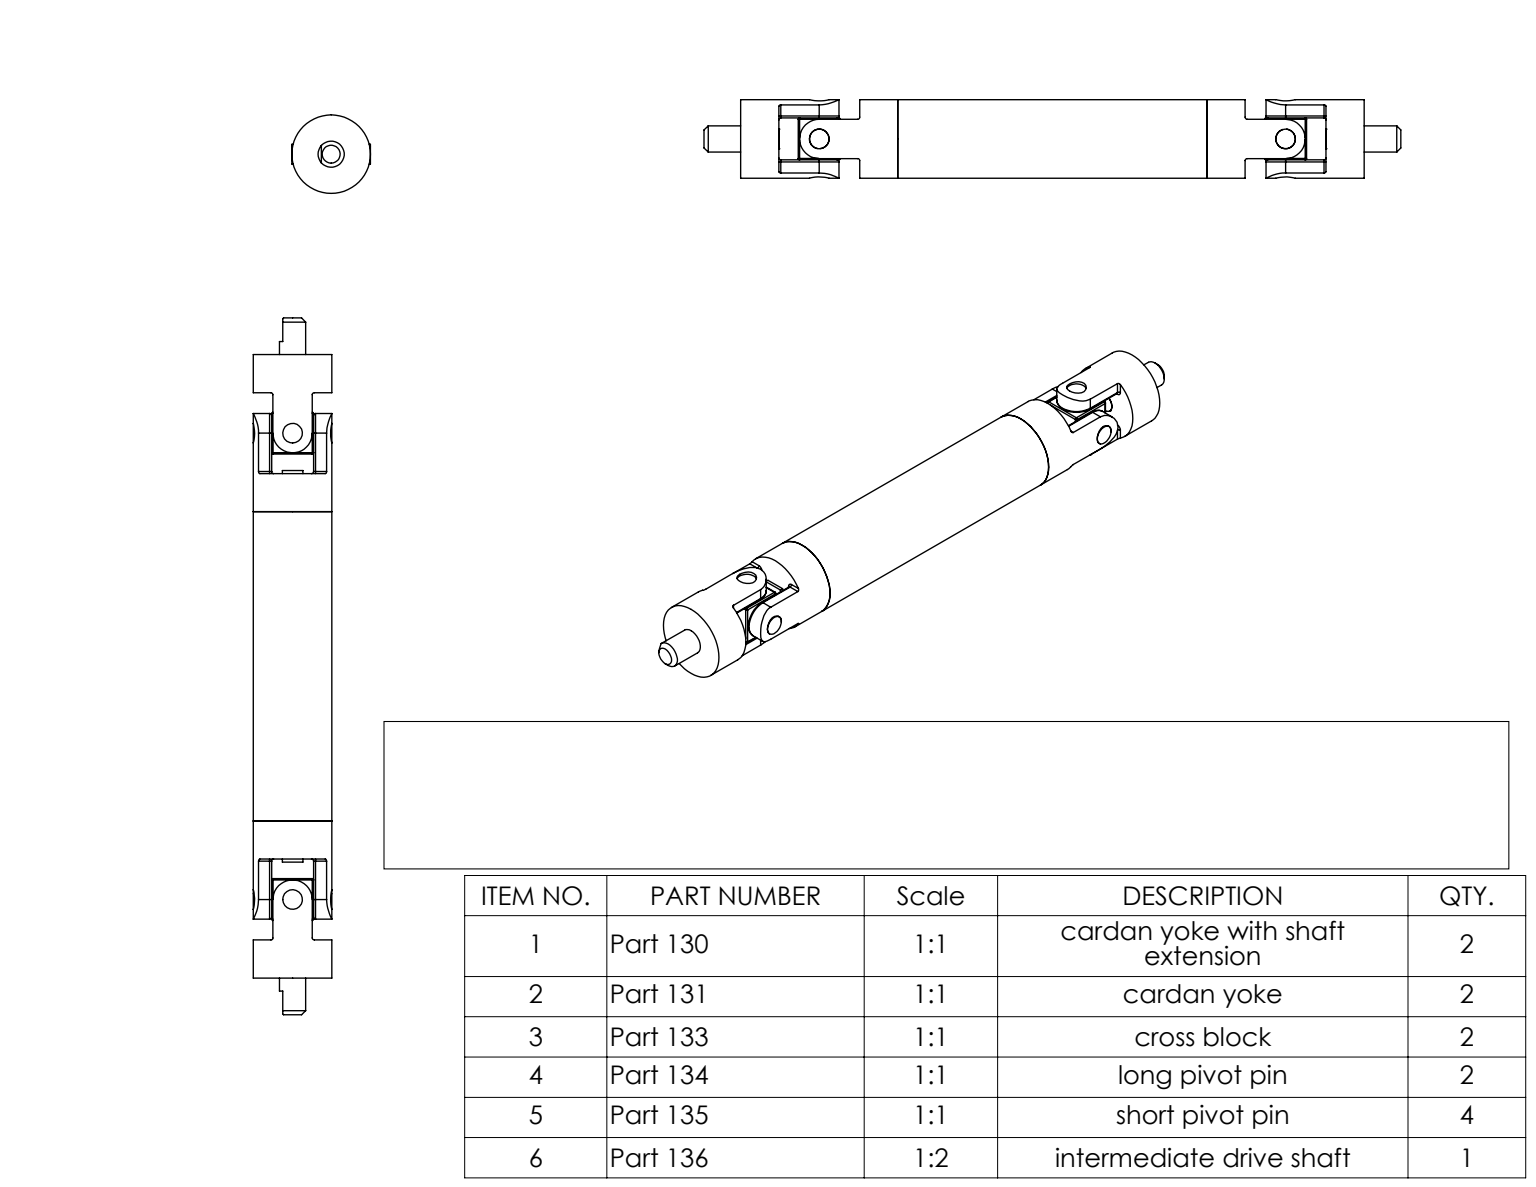
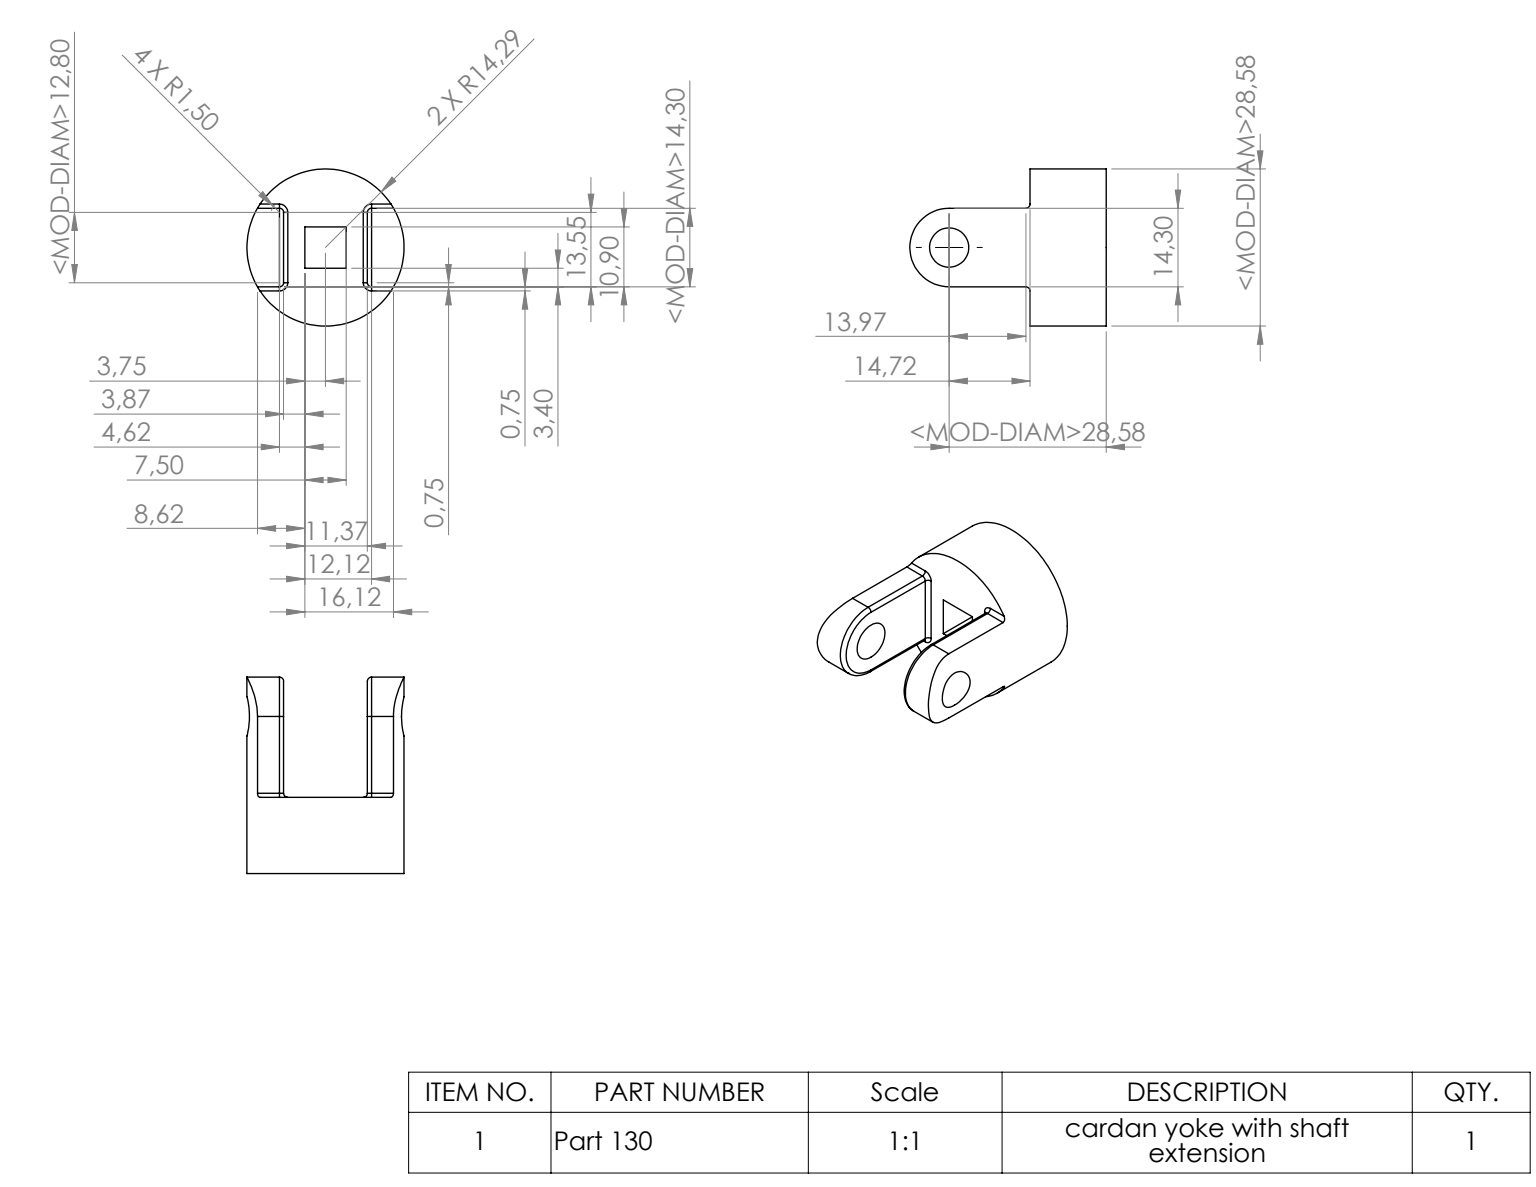
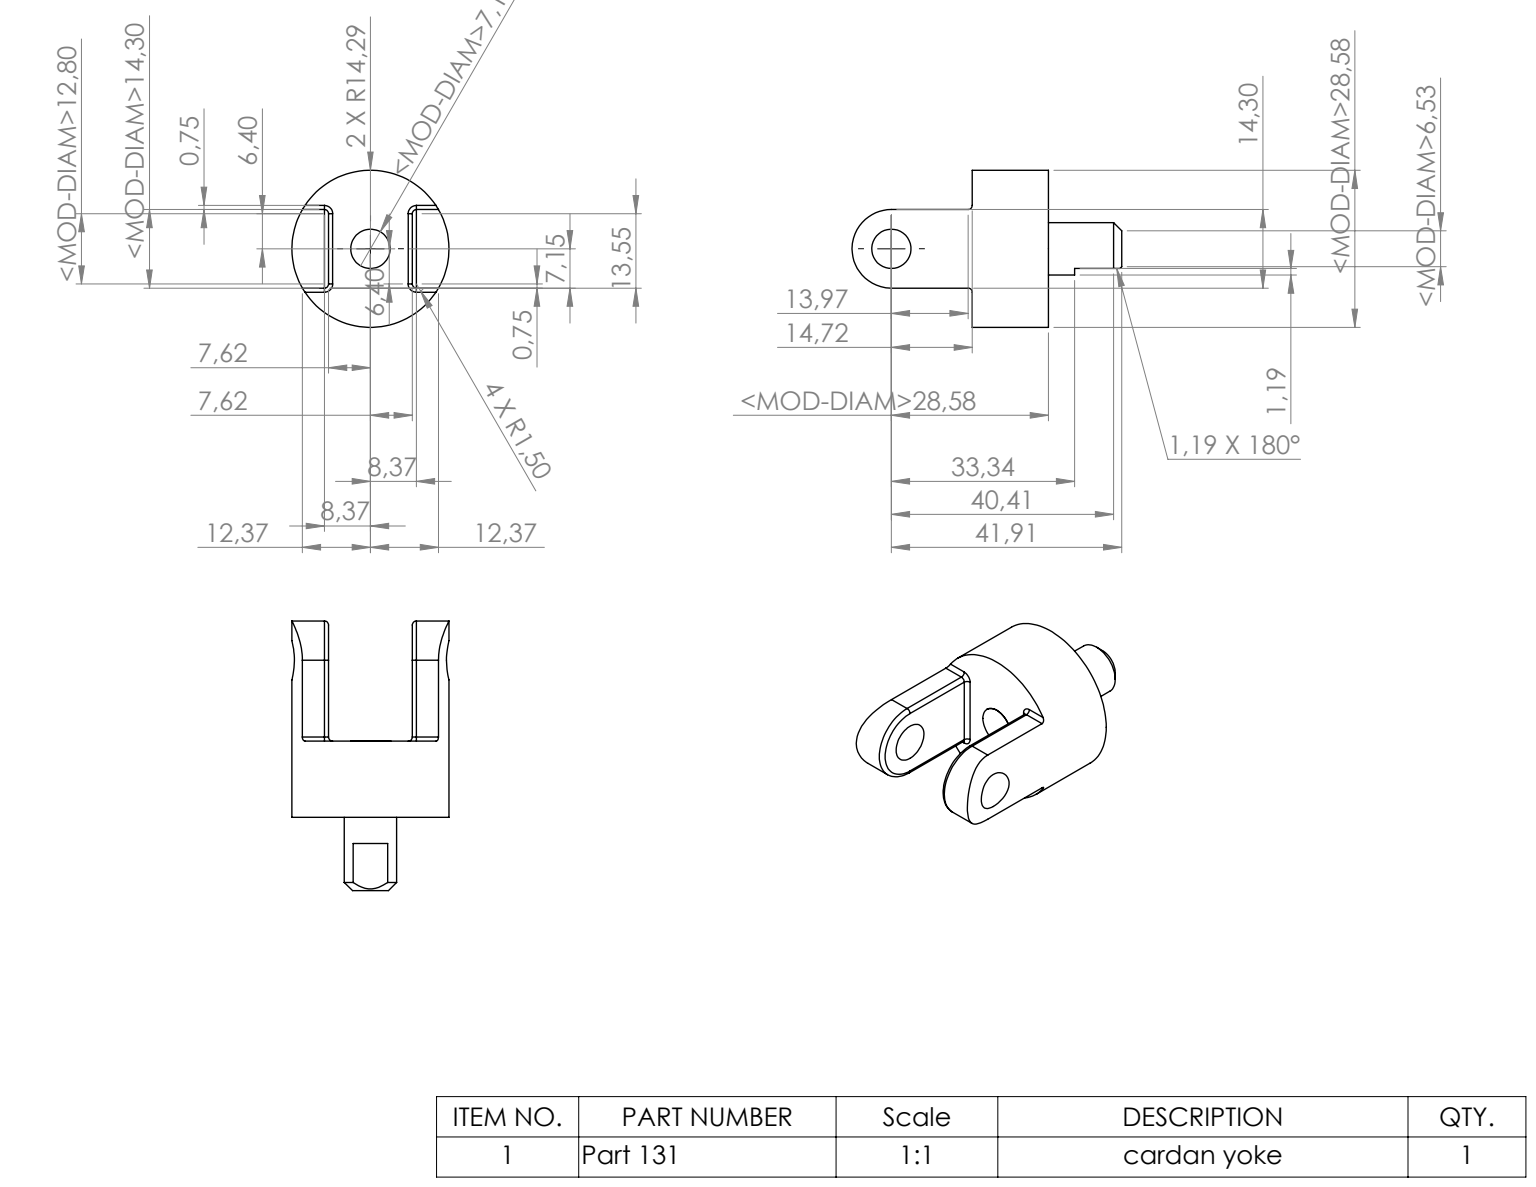
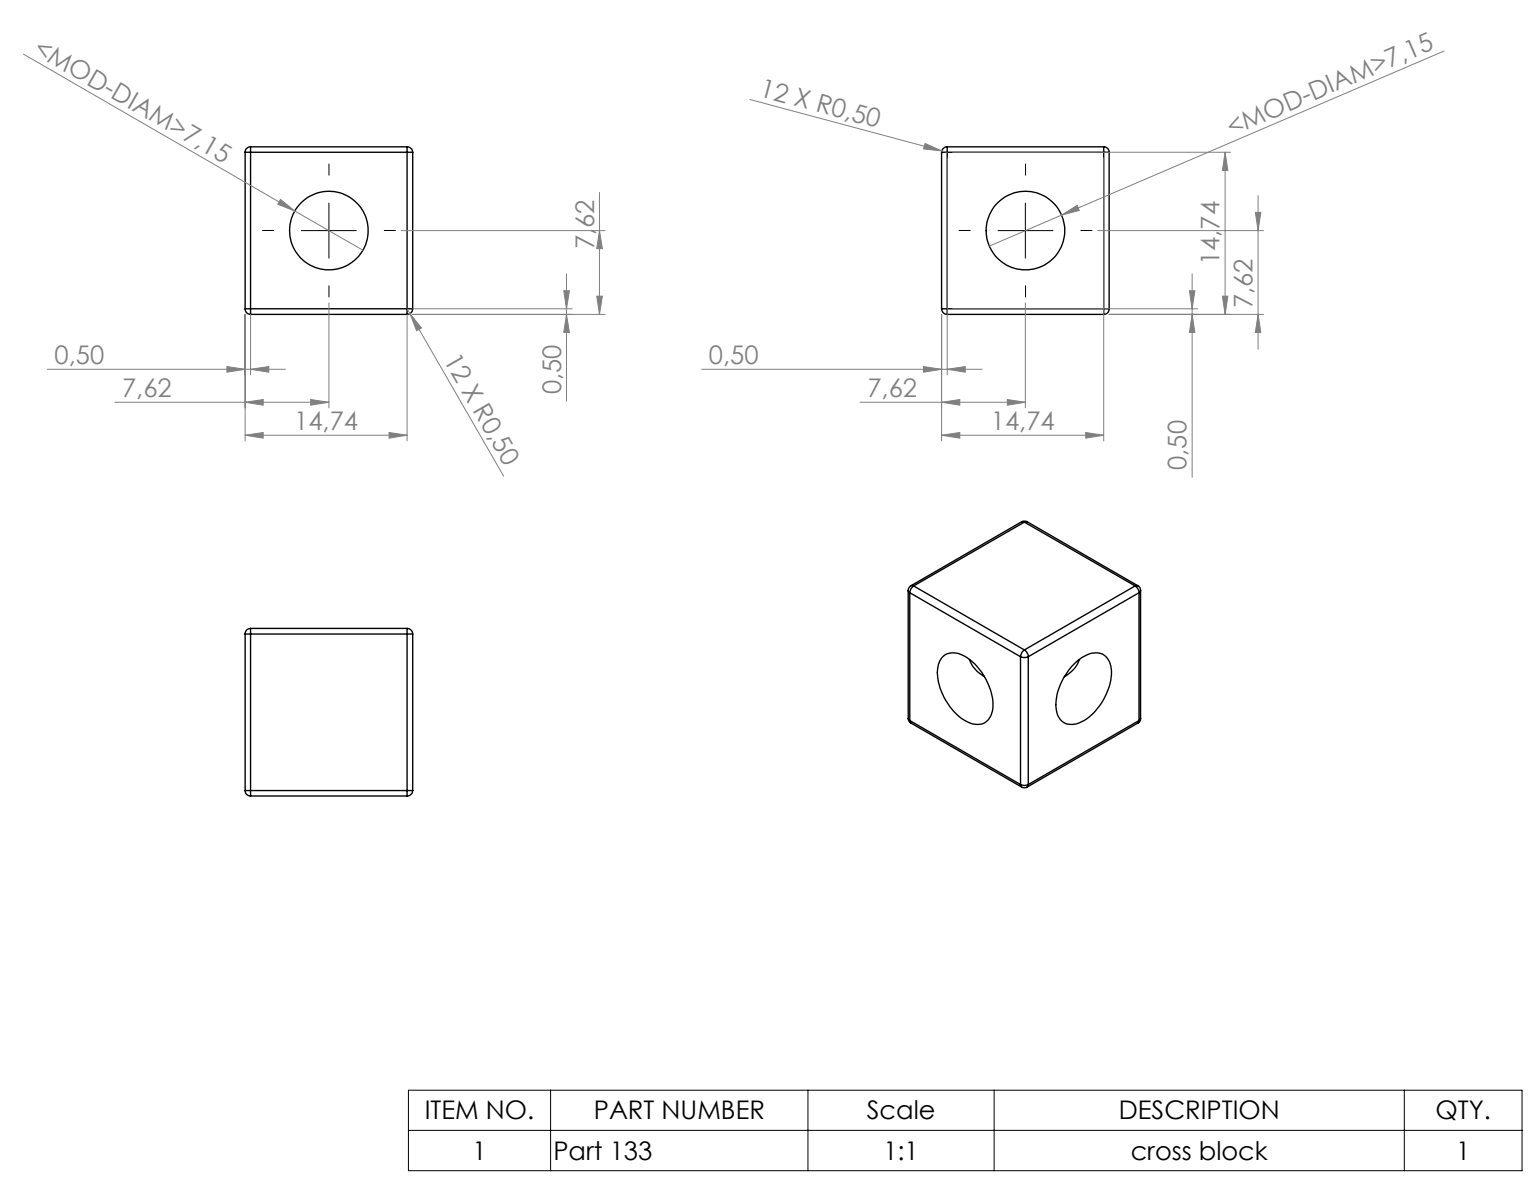
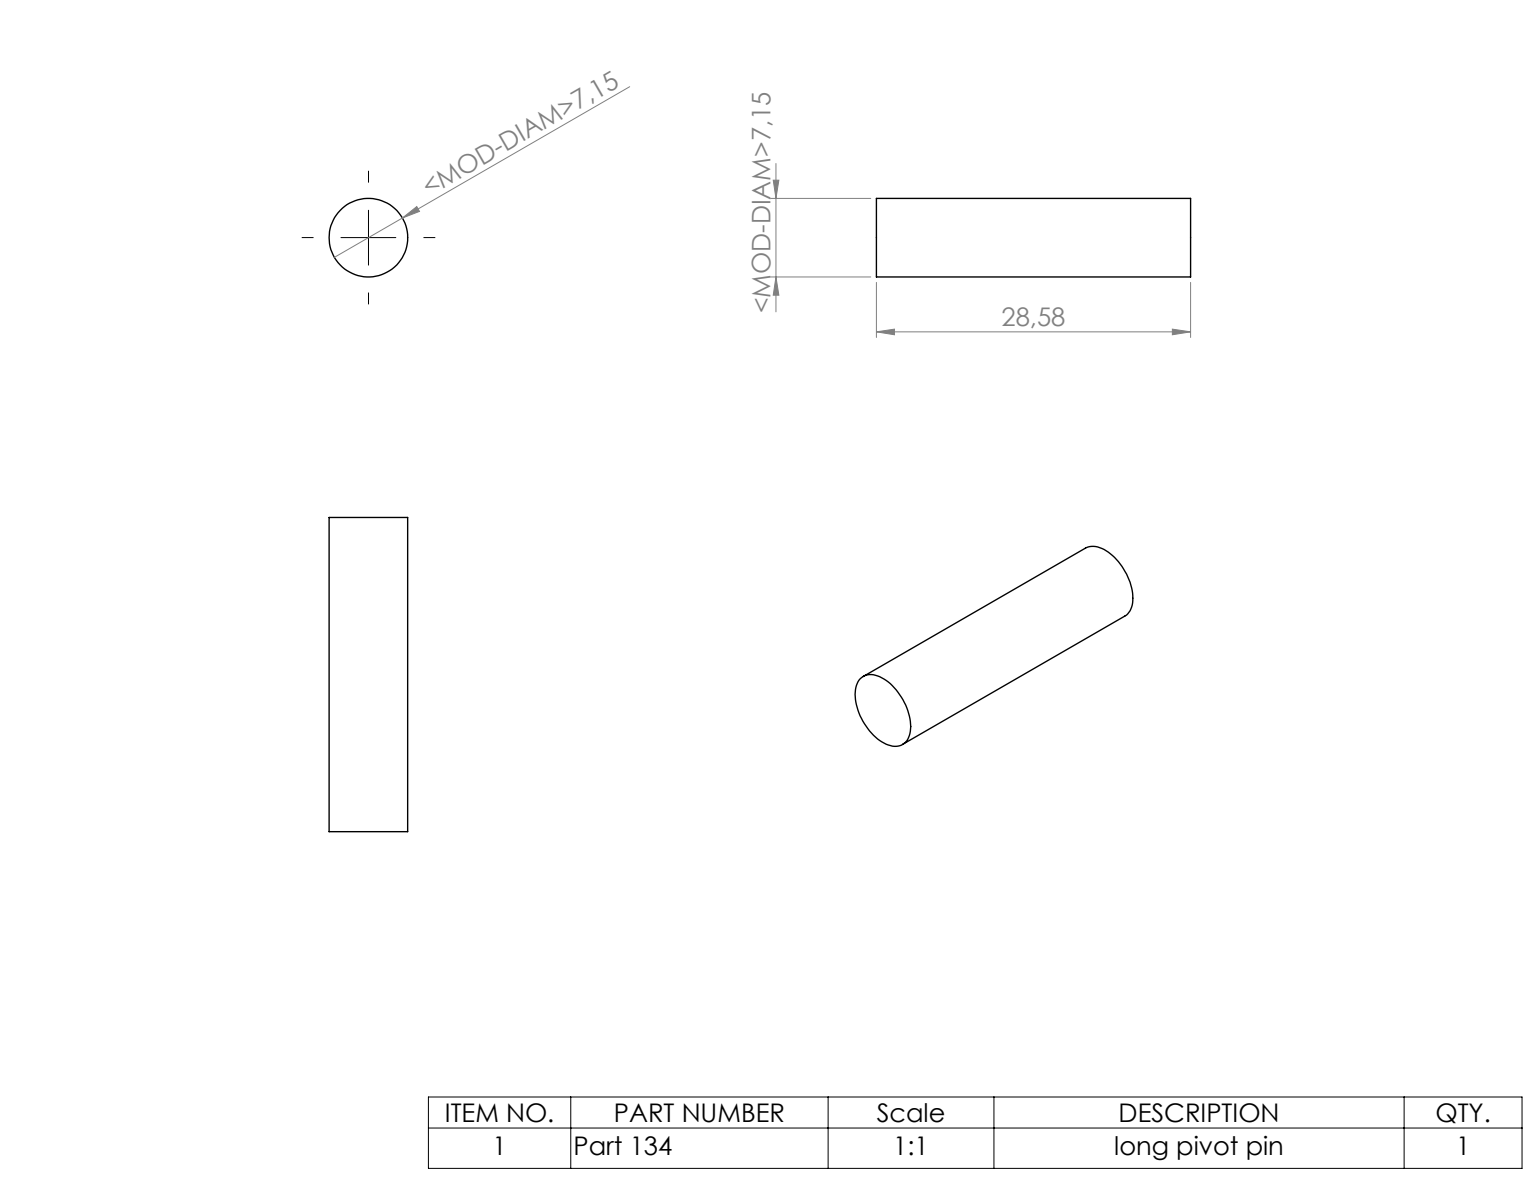
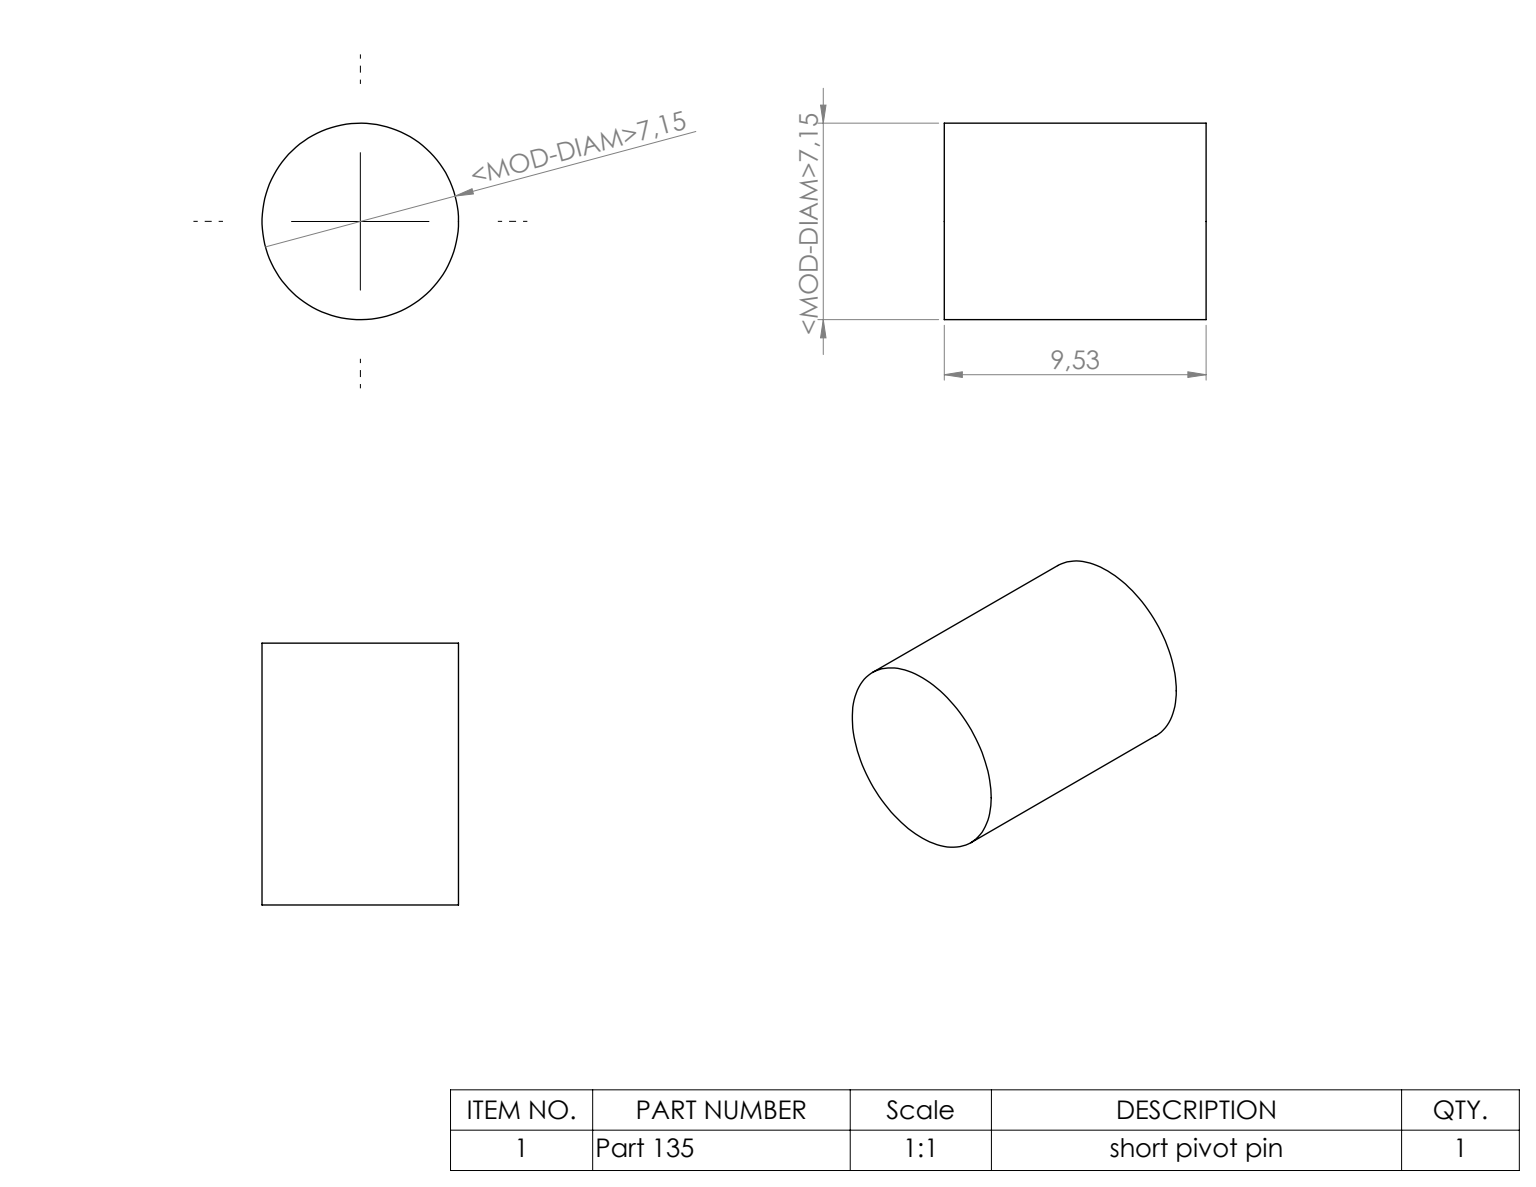
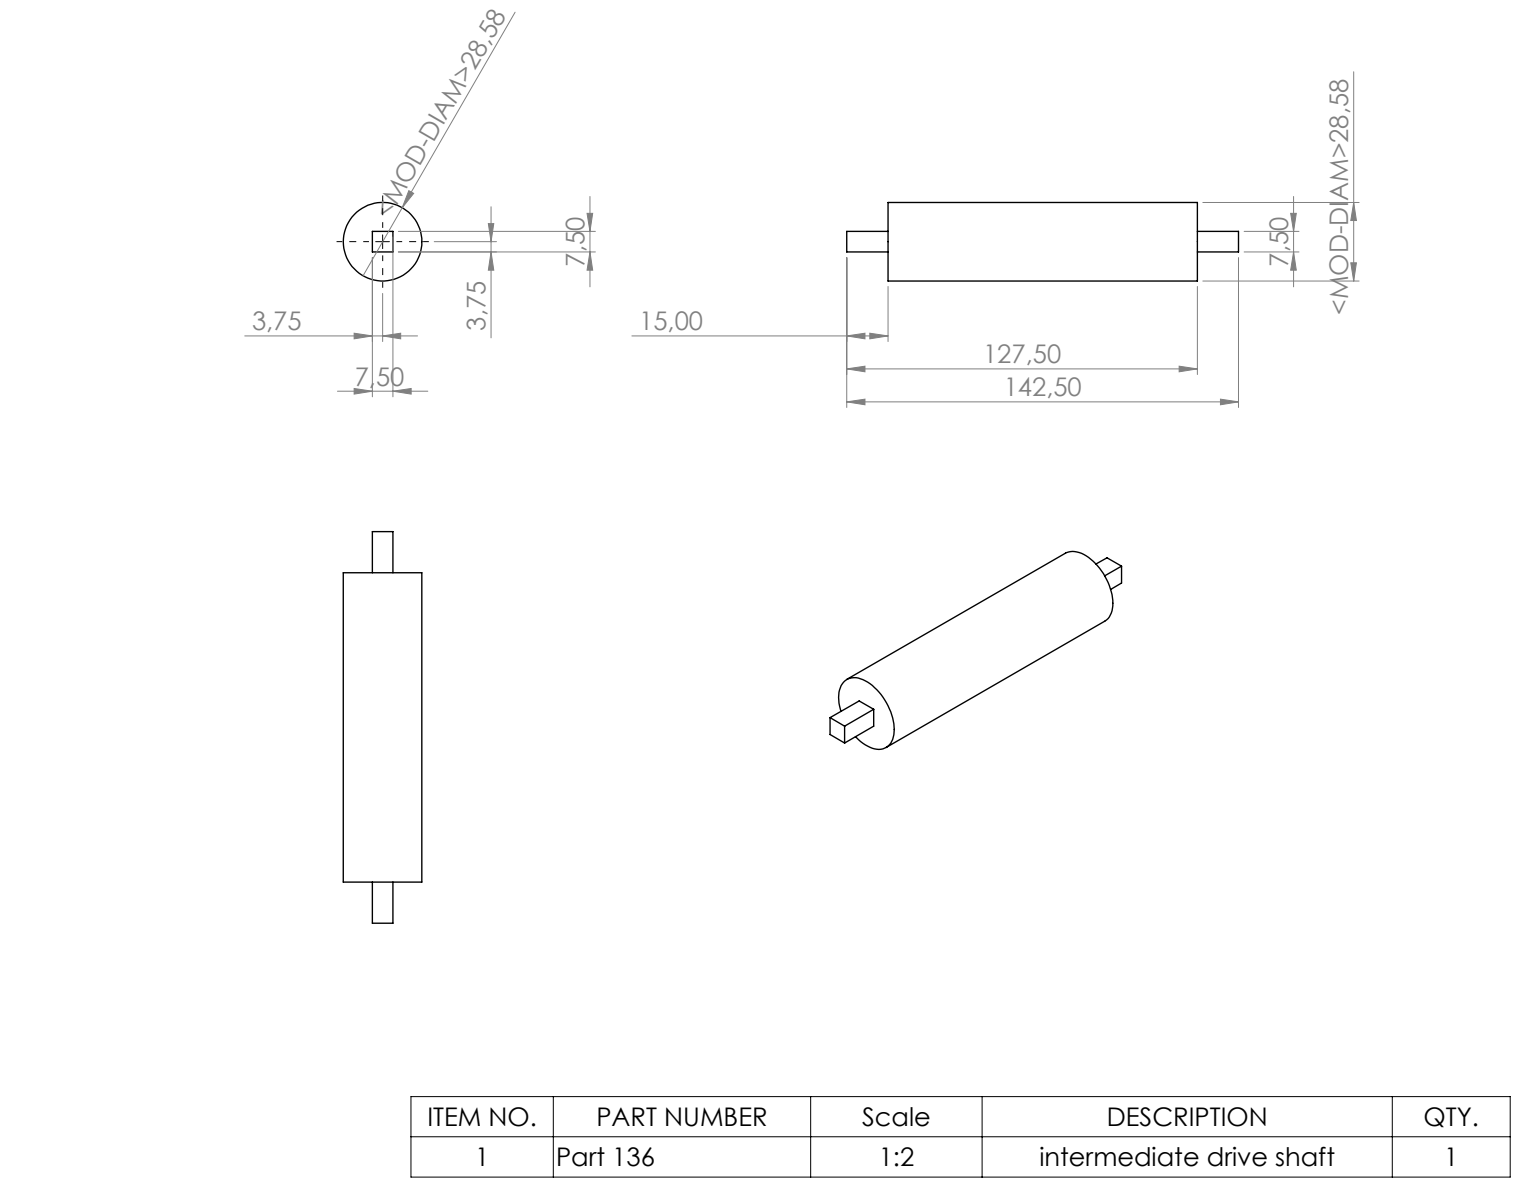
ISO-10303-21;
HEADER;
FILE_DESCRIPTION (('STEP AP214'),
    '1' );
FILE_NAME ('MAS-681',
    '2026-10-08T11:03:28',
    ( '' ),
    ( '' ),
    'SwSTEP 2.0',
    'SolidWorks 2024',
    '' );
FILE_SCHEMA (( 'AUTOMOTIVE_DESIGN' ));
ENDSEC;

DATA;
#1 = ORIENTED_EDGE ( 'NONE', *, *, #3804, .F. ) ;
#2 = CARTESIAN_POINT ( 'NONE',  ( -13.11668479459951087, 5.670681919514632519, 36.22991310522757402 ) ) ;
#3 = ORIENTED_EDGE ( 'NONE', *, *, #1718, .F. ) ;
#4 = VERTEX_POINT ( 'NONE', #1586 ) ;
#5 = DIRECTION ( 'NONE',  ( -0.000000000000000000, -0.000000000000000000, -1.000000000000000000 ) ) ;
#6 = CARTESIAN_POINT ( 'NONE',  ( -8.423108025121079478, 3.330708927240789485, -103.6440396064643323 ) ) ;
#7 = VECTOR ( 'NONE', #913, 1000.000000000000000 ) ;
#8 = LINE ( 'NONE', #2469, #3092 ) ;
#9 = VECTOR ( 'NONE', #126, 1000.000000000000000 ) ;
#10 = CARTESIAN_POINT ( 'NONE',  ( 8.370007234561949616, 7.901597986548672736, 17.90262445358908039 ) ) ;
#11 = CARTESIAN_POINT ( 'NONE',  ( 12.37117936981251631, 7.901597986548669184, 17.15262445358908039 ) ) ;
#12 = PLANE ( 'NONE',  #3351 ) ;
#13 = EDGE_CURVE ( 'NONE', #1212, #3737, #2435, .T. ) ;
#14 = PRODUCT_DEFINITION ( 'UNKNOWN', '', #194, #518 ) ;
#15 = CYLINDRICAL_SURFACE ( 'NONE', #4136, 0.7500000000000006661 ) ;
#16 = CYLINDRICAL_SURFACE ( 'NONE', #1372, 0.7499999999999997780 ) ;
#17 = FILL_AREA_STYLE_COLOUR ( '', #4215 ) ;
#18 = AXIS2_PLACEMENT_3D ( 'NONE', #23, #1540, #3973 ) ;
#19 = CARTESIAN_POINT ( 'NONE',  ( 11.96600549393350299, -7.807631214078937454, 17.65096039353564805 ) ) ;
#20 = EDGE_CURVE ( 'NONE', #2372, #3471, #3030, .T. ) ;
#21 = VERTEX_POINT ( 'NONE', #4097 ) ;
#22 = DIRECTION ( 'NONE',  ( 1.000000000000000000, 1.076498916035107621E-16, -0.000000000000000000 ) ) ;
#23 = CARTESIAN_POINT ( 'NONE',  ( -6.869994990996021400, -6.397499167952784838, 18.40096039353565160 ) ) ;
#24 = DIRECTION ( 'NONE',  ( 0.000000000000000000, 1.000000000000000000, 0.000000000000000000 ) ) ;
#25 = ORIENTED_EDGE ( 'NONE', *, *, #871, .F. ) ;
#26 = EDGE_LOOP ( 'NONE', ( #2589, #425, #54, #3081 ) ) ;
#27 = CARTESIAN_POINT ( 'NONE',  ( -12.39927918895608094, 7.103532125216092119, 32.82105853334656587 ) ) ;
#28 = AXIS2_PLACEMENT_3D ( 'NONE', #4115, #895, #1519 ) ;
#29 = EDGE_LOOP ( 'NONE', ( #1981, #2414, #2943, #1041 ) ) ;
#30 = ORIENTED_EDGE ( 'NONE', *, *, #51, .F. ) ;
#31 = DIRECTION ( 'NONE',  ( -1.076498916035107621E-16, -1.000000000000000000, -8.841607930564763213E-17 ) ) ;
#32 = ADVANCED_FACE ( 'NONE', ( #797 ), #4451, .F. ) ;
#33 = DIRECTION ( 'NONE',  ( 3.602528553751907911E-16, -0.8113431300520737022, 0.5845702056359901588 ) ) ;
#34 = CARTESIAN_POINT ( 'NONE',  ( -0.2830874312243520929, -3.565902013451327512, -9.735057145307090209 ) ) ;
#35 = CARTESIAN_POINT ( 'NONE',  ( 3.749999999999999556, 3.750000000000000000, 3.749999999999995559 ) ) ;
#36 = EDGE_CURVE ( 'NONE', #2260, #2464, #1685, .T. ) ;
#37 = DIRECTION ( 'NONE',  ( 0.000000000000000000, -8.673617379884027583E-16, 1.000000000000000000 ) ) ;
#38 = DIRECTION ( 'NONE',  ( -0.000000000000000000, -0.000000000000000000, -1.000000000000000000 ) ) ;
#39 = EDGE_CURVE ( 'NONE', #3048, #992, #3247, .T. ) ;
#40 = DIRECTION ( 'NONE',  ( 0.000000000000000000, 1.000000000000000000, 0.000000000000000000 ) ) ;
#41 = DIRECTION ( 'NONE',  ( 0.000000000000000000, 1.000000000000000000, 0.000000000000000000 ) ) ;
#42 =( NAMED_UNIT ( * ) SI_UNIT ( $, .STERADIAN. ) SOLID_ANGLE_UNIT ( ) );
#43 = PLANE ( 'NONE',  #271 ) ;
#44 = VERTEX_POINT ( 'NONE', #445 ) ;
#45 = CARTESIAN_POINT ( 'NONE',  ( 14.28750500900398279, 8.320472145597748469E-07, 17.65096039353565160 ) ) ;
#46 = DIRECTION ( 'NONE',  ( 1.000000000000000000, -8.673617379884027583E-16, 0.000000000000000000 ) ) ;
#47 = PLANE ( 'NONE',  #853 ) ;
#48 = ORIENTED_EDGE ( 'NONE', *, *, #4168, .T. ) ;
#49 = VECTOR ( 'NONE', #2598, 1000.000000000000000 ) ;
#50 = ORIENTED_EDGE ( 'NONE', *, *, #62, .T. ) ;
#51 = EDGE_CURVE ( 'NONE', #1305, #4402, #2822, .T. ) ;
#52 = SURFACE_SIDE_STYLE ('',( #3578 ) ) ;
#53 = ORIENTED_EDGE ( 'NONE', *, *, #4114, .T. ) ;
#54 = ORIENTED_EDGE ( 'NONE', *, *, #659, .F. ) ;
#55 = DIRECTION ( 'NONE',  ( -0.000000000000000000, -0.000000000000000000, -1.000000000000000000 ) ) ;
#56 = APPLICATION_PROTOCOL_DEFINITION ( 'draft international standard', 'automotive_design', 1998, #2013 ) ;
#57 = EDGE_CURVE ( 'NONE', #1869, #1513, #3978, .T. ) ;
#58 = CARTESIAN_POINT ( 'NONE',  ( 12.76962931635276455, 6.415859468635933816, 35.06035830646958829 ) ) ;
#59 = EDGE_CURVE ( 'NONE', #4262, #44, #387, .T. ) ;
#60 = CARTESIAN_POINT ( 'NONE',  ( -14.12140203323284204, 2.180955620240156545, 29.52533606476202621 ) ) ;
#61 = CARTESIAN_POINT ( 'NONE',  ( 6.870007234561953169, -6.393402013451325416, 17.15262445358908039 ) ) ;
#62 = EDGE_CURVE ( 'NONE', #3737, #4361, #8, .T. ) ;
#63 = CARTESIAN_POINT ( 'NONE',  ( -8.369992765438043492, 6.401597986548673624, 17.90262445358908039 ) ) ;
#64 = SPHERICAL_SURFACE ( 'NONE', #81, 0.5000000000000000000 ) ;
#65 = FACE_OUTER_BOUND ( 'NONE', #1668, .T. ) ;
#66 = ORIENTED_EDGE ( 'NONE', *, *, #2001, .F. ) ;
#67 = CARTESIAN_POINT ( 'NONE',  ( -17.48249499099600968, -7.897499167952782173, 18.40096039353565160 ) ) ;
#68 = FACE_OUTER_BOUND ( 'NONE', #2702, .T. ) ;
#69 = AXIS2_PLACEMENT_3D ( 'NONE', #833, #180, #3017 ) ;
#70 = CARTESIAN_POINT ( 'NONE',  ( -8.369994990996016071, 6.397500832047212427, 17.65096039353565160 ) ) ;
#71 =( BOUNDED_CURVE ( )  B_SPLINE_CURVE ( 3, ( #2713, #202, #1737, #3164 ),
 .UNSPECIFIED., .F., .F. ) 
 B_SPLINE_CURVE_WITH_KNOTS ( ( 4, 4 ),
 ( 0.000000000000000000, 1.570796326794896558 ),
 .UNSPECIFIED. ) 
 CURVE ( )  GEOMETRIC_REPRESENTATION_ITEM ( )  RATIONAL_B_SPLINE_CURVE ( ( 1.000000000000000000, 0.8047378541243649375, 0.8047378541243649375, 1.000000000000000000 ) ) 
 REPRESENTATION_ITEM ( '' )  );
#72 = EDGE_CURVE ( 'NONE', #4385, #2774, #2483, .T. ) ;
#73 = ORIENTED_EDGE ( 'NONE', *, *, #84, .T. ) ;
#74 = CARTESIAN_POINT ( 'NONE',  ( -12.37116490068861019, 7.151597986548670072, 17.90262445358908039 ) ) ;
#75 = DIRECTION ( 'NONE',  ( -1.000000000000000000, -0.000000000000000000, -0.000000000000000000 ) ) ;
#76 = ORIENTED_EDGE ( 'NONE', *, *, #1333, .T. ) ;
#77 = ORIENTED_EDGE ( 'NONE', *, *, #3651, .T. ) ;
#78 = DIRECTION ( 'NONE',  ( 0.000000000000000000, 0.000000000000000000, -1.000000000000000000 ) ) ;
#79 = ITEM_DEFINED_TRANSFORMATION ( 'NONE', 'NONE', #4173,  #4483 ) ;
#80 = CARTESIAN_POINT ( 'NONE',  ( 13.92256467935009034, -3.209909955418536409, 30.77756777369077312 ) ) ;
#81 = AXIS2_PLACEMENT_3D ( 'NONE', #3592, #41, #3309 ) ;
#82 = CARTESIAN_POINT ( 'NONE',  ( 6.586250505521797471, -10.16000000000000014, 17.78000050552179445 ) ) ;
#83 = MECHANICAL_DESIGN_GEOMETRIC_PRESENTATION_REPRESENTATION (  '', ( #914 ), #4064 ) ;
#84 = EDGE_CURVE ( 'NONE', #2363, #3745, #1077, .T. ) ;
#85 = DIRECTION ( 'NONE',  ( 0.000000000000000000, 0.000000000000000000, 1.000000000000000000 ) ) ;
#86 = CARTESIAN_POINT ( 'NONE',  ( 17.28000050552179800, -17.28000000000000114, 17.78000050552179445 ) ) ;
#87 = AXIS2_PLACEMENT_3D ( 'NONE', #761, #3633, #4319 ) ;
#88 = DIRECTION ( 'NONE',  ( -0.000000000000000000, -0.000000000000000000, -1.000000000000000000 ) ) ;
#89 = SPHERICAL_SURFACE ( 'NONE', #874, 0.5000000000000000000 ) ;
#90 = ADVANCED_FACE ( 'NONE', ( #3987 ), #2494, .T. ) ;
#91 = ORIENTED_EDGE ( 'NONE', *, *, #2174, .T. ) ;
#92 = DIRECTION ( 'NONE',  ( 1.707404996040164265E-16, -1.000000000000000000, 0.000000000000000000 ) ) ;
#93 = CYLINDRICAL_SURFACE ( 'NONE', #677, 3.573749999999999538 ) ;
#94 = ORIENTED_EDGE ( 'NONE', *, *, #395, .F. ) ;
#95 = DIRECTION ( 'NONE',  ( 1.076498916035107621E-16, 1.000000000000000000, -0.000000000000000000 ) ) ;
#96 = ORIENTED_EDGE ( 'NONE', *, *, #3980, .T. ) ;
#97 = CARTESIAN_POINT ( 'NONE',  ( 14.99250723456195544, 7.901597986548669184, 17.90262445358908039 ) ) ;
#98 = VERTEX_POINT ( 'NONE', #430 ) ;
#99 = ORIENTED_EDGE ( 'NONE', *, *, #1933, .F. ) ;
#100 = DIRECTION ( 'NONE',  ( 0.000000000000000000, 1.000000000000000000, -0.000000000000000000 ) ) ;
#101 = AXIS2_PLACEMENT_3D ( 'NONE', #3470, #3879, #4145 ) ;
#102 = CARTESIAN_POINT ( 'NONE',  ( -12.18302349840153731, -7.460057201642745106, 17.28264009582346006 ) ) ;
#103 = EDGE_LOOP ( 'NONE', ( #548, #3228, #3814, #302 ) ) ;
#104 = DIRECTION ( 'NONE',  ( 0.000000000000000000, 1.000000000000000000, -0.000000000000000000 ) ) ;
#105 = EDGE_CURVE ( 'NONE', #338, #3364, #3317, .T. ) ;
#106 = CARTESIAN_POINT ( 'NONE',  ( -7.619992765438047044, -7.143402013451323640, 17.90262445358908039 ) ) ;
#107 = DIRECTION ( 'NONE',  ( 0.000000000000000000, 0.000000000000000000, 1.000000000000000000 ) ) ;
#108 = LINE ( 'NONE', #835, #4367 ) ;
#109 = CARTESIAN_POINT ( 'NONE',  ( 10.16000050552179701, -10.16000000000000014, 17.78000050552179445 ) ) ;
#110 = ORIENTED_EDGE ( 'NONE', *, *, #3169, .F. ) ;
#111 = CARTESIAN_POINT ( 'NONE',  ( 8.370007234561953169, 7.151597986548671848, 17.90262445358908039 ) ) ;
#112 = DIRECTION ( 'NONE',  ( -8.673617379884035472E-17, 1.000000000000000000, -0.000000000000000000 ) ) ;
#113 = EDGE_CURVE ( 'NONE', #3745, #2828, #2285, .T. ) ;
#114 = EDGE_CURVE ( 'NONE', #4543, #2437, #498, .T. ) ;
#115 = CARTESIAN_POINT ( 'NONE',  ( 6.870005009003977037, -6.397499167952786614, 18.40096039353565160 ) ) ;
#116 = VERTEX_POINT ( 'NONE', #479 ) ;
#117 = CARTESIAN_POINT ( 'NONE',  ( 13.94777217564051952, -3.095918481782248044, 30.07429697042405081 ) ) ;
#118 = DIRECTION ( 'NONE',  ( 0.000000000000000000, 0.000000000000000000, -1.000000000000000000 ) ) ;
#119 = AXIS2_PLACEMENT_3D ( 'NONE', #3333, #3405, #2246 ) ;
#120 = EDGE_CURVE ( 'NONE', #4361, #2188, #836, .T. ) ;
#121 = CARTESIAN_POINT ( 'NONE',  ( 13.83333536583607959, 3.577847986548670978, 31.86762445358909446 ) ) ;
#122 = EDGE_LOOP ( 'NONE', ( #2207, #3885, #1345, #218 ) ) ;
#123 = EDGE_CURVE ( 'NONE', #2304, #1592, #1177, .T. ) ;
#124 = ORIENTED_EDGE ( 'NONE', *, *, #4476, .F. ) ;
#125 = CONTEXT_DEPENDENT_SHAPE_REPRESENTATION ( #141, #3032 ) ;
#126 = DIRECTION ( 'NONE',  ( -0.000000000000000000, -0.000000000000000000, -1.000000000000000000 ) ) ;
#127 = ORIENTED_EDGE ( 'NONE', *, *, #123, .T. ) ;
#128 = CIRCLE ( 'NONE', #4565, 6.397499999999999964 ) ;
#129 = DIRECTION ( 'NONE',  ( 0.000000000000000000, 0.000000000000000000, 1.000000000000000000 ) ) ;
#130 = DIRECTION ( 'NONE',  ( -0.000000000000000000, -0.000000000000000000, -1.000000000000000000 ) ) ;
#131 = CARTESIAN_POINT ( 'NONE',  ( -13.83927268380397635, 3.555046762887689837, 32.33443371951124590 ) ) ;
#132 = CARTESIAN_POINT ( 'NONE',  ( 7.234561953626996335E-06, 0.004097986548672528061, -1.469875546410923661 ) ) ;
#133 = ORIENTED_EDGE ( 'NONE', *, *, #4375, .F. ) ;
#134 = PLANE ( 'NONE',  #2161 ) ;
#135 = FACE_OUTER_BOUND ( 'NONE', #1112, .T. ) ;
#136 = AXIS2_PLACEMENT_3D ( 'NONE', #1284, #2724, #2568 ) ;
#137 = DIRECTION ( 'NONE',  ( -1.000000000000000000, 0.000000000000000000, 0.000000000000000000 ) ) ;
#138 = ORIENTED_EDGE ( 'NONE', *, *, #1516, .F. ) ;
#139 = CARTESIAN_POINT ( 'NONE',  ( 12.25345478699094670, -6.586249999999999716, 12.25345478699094670 ) ) ;
#140 = ORIENTED_EDGE ( 'NONE', *, *, #3397, .F. ) ;
#141 =( REPRESENTATION_RELATIONSHIP ('NONE','NONE', #4401, #2796 ) REPRESENTATION_RELATIONSHIP_WITH_TRANSFORMATION ( #496 )SHAPE_REPRESENTATION_RELATIONSHIP( ) );
#142 = DIRECTION ( 'NONE',  ( 1.000000000000000000, -1.076498916035107744E-16, 0.000000000000000000 ) ) ;
#143 = CARTESIAN_POINT ( 'NONE',  ( 13.83333536583607959, 3.577847986548671422, 32.33516565723597580 ) ) ;
#144 = PRODUCT_DEFINITION_SHAPE ( 'NONE', 'NONE',  #4662 ) ;
#145 = ORIENTED_EDGE ( 'NONE', *, *, #329, .T. ) ;
#146 = ORIENTED_EDGE ( 'NONE', *, *, #3284, .F. ) ;
#147 = ITEM_DEFINED_TRANSFORMATION ( 'NONE', 'NONE', #1851,  #4483 ) ;
#148 = CARTESIAN_POINT ( 'NONE',  ( -12.02318935820893664, -7.715086390250210258, 17.16832378532598113 ) ) ;
#149 = CIRCLE ( 'NONE', #1518, 0.7500000000000006661 ) ;
#150 = ORIENTED_EDGE ( 'NONE', *, *, #1875, .T. ) ;
#151 = CARTESIAN_POINT ( 'NONE',  ( 12.37117936981251987, 7.151597986548668295, 17.90262445358908039 ) ) ;
#152 = DIRECTION ( 'NONE',  ( 8.673617379884035472E-17, 1.000000000000000000, 0.000000000000000000 ) ) ;
#153 = LINE ( 'NONE', #555, #974 ) ;
#154 = VECTOR ( 'NONE', #4373, 1000.000000000000000 ) ;
#155 = DIRECTION ( 'NONE',  ( -1.000000000000000000, 1.076498916035107744E-16, 0.000000000000000000 ) ) ;
#156 = CARTESIAN_POINT ( 'NONE',  ( -12.27094704565411121, 7.318711406274640119, 17.91402383463540104 ) ) ;
#157 = ORIENTED_EDGE ( 'NONE', *, *, #1855, .F. ) ;
#158 = EDGE_CURVE ( 'NONE', #2359, #3396, #1229, .T. ) ;
#159 = EDGE_CURVE ( 'NONE', #3907, #1168, #3927, .T. ) ;
#160 = CYLINDRICAL_SURFACE ( 'NONE', #3367, 3.573749999999999538 ) ;
#161 = ADVANCED_BREP_SHAPE_REPRESENTATION ( '', ( #1920, #4483 ), #2891 ) ;
#162 = CIRCLE ( 'NONE', #2984, 0.7500000000000006661 ) ;
#163 = EDGE_CURVE ( 'NONE', #696, #4208, #4390, .T. ) ;
#164 = VECTOR ( 'NONE', #2575, 1000.000000000000000 ) ;
#165 = CARTESIAN_POINT ( 'NONE',  ( 13.94792900051583651, 3.103387315081731934, 30.07316051872297535 ) ) ;
#166 = EDGE_CURVE ( 'NONE', #1497, #1208, #805, .T. ) ;
#167 = ORIENTED_EDGE ( 'NONE', *, *, #3789, .T. ) ;
#168 = DIRECTION ( 'NONE',  ( 0.000000000000000000, -1.000000000000000000, 0.000000000000000000 ) ) ;
#169 = CARTESIAN_POINT ( 'NONE',  ( -14.28749499099602005, 0.2372044551111577027, 35.93971039353565544 ) ) ;
#170 = CARTESIAN_POINT ( 'NONE',  ( -3.749999999999999556, -3.750000000000000888, 131.2499999999999716 ) ) ;
#171 = ORIENTED_EDGE ( 'NONE', *, *, #591, .T. ) ;
#172 = ORIENTED_EDGE ( 'NONE', *, *, #2866, .T. ) ;
#173 = ITEM_DEFINED_TRANSFORMATION ( 'NONE', 'NONE', #491,  #4483 ) ;
#174 = CARTESIAN_POINT ( 'NONE',  ( 13.92220474334306601, 3.211459441160700923, 30.78080196879686170 ) ) ;
#175 = CARTESIAN_POINT ( 'NONE',  ( 8.370007234561949616, -7.893402013451324528, 17.90262445358908039 ) ) ;
#176 = EDGE_LOOP ( 'NONE', ( #2140, #3817, #1217, #3827 ) ) ;
#177 = EDGE_CURVE ( 'NONE', #3571, #1450, #388, .T. ) ;
#178 = CIRCLE ( 'NONE', #3931, 3.573749999999998650 ) ;
#179 = CARTESIAN_POINT ( 'NONE',  ( 10.16000050552179701, -6.586249999999999716, 10.16000050552179701 ) ) ;
#180 = DIRECTION ( 'NONE',  ( 0.000000000000000000, 0.000000000000000000, -1.000000000000000000 ) ) ;
#181 = CARTESIAN_POINT ( 'NONE',  ( -14.09151123534772765, 2.368322898672384991, 34.55761253202872041 ) ) ;
#182 = CARTESIAN_POINT ( 'NONE',  ( 8.370007234561954945, -7.143402013451326305, 31.86762445358908735 ) ) ;
#183 = EDGE_CURVE ( 'NONE', #3678, #2227, #613, .T. ) ;
#184 = ORIENTED_EDGE ( 'NONE', *, *, #3116, .F. ) ;
#185 = EDGE_CURVE ( 'NONE', #3472, #4004, #3811, .T. ) ;
#186 = CARTESIAN_POINT ( 'NONE',  ( 17.28000050552179445, -3.039999999999999591, 17.28000050552179445 ) ) ;
#187 = EDGE_LOOP ( 'NONE', ( #3, #2637, #1708, #1494 ) ) ;
#188 = FACE_OUTER_BOUND ( 'NONE', #2341, .T. ) ;
#189 = PRODUCT_DEFINITION_SHAPE ( 'NONE', 'NONE',  #4658 ) ;
#190 = ORIENTED_EDGE ( 'NONE', *, *, #2135, .T. ) ;
#191 = CARTESIAN_POINT ( 'NONE',  ( -13.86254577222764262, 3.458987924946582915, 33.29469953564710494 ) ) ;
#192 = CARTESIAN_POINT ( 'NONE',  ( 12.37117714425454551, -7.147499167952784838, 18.40096039353565160 ) ) ;
#193 = DIRECTION ( 'NONE',  ( -1.000000000000000000, -0.000000000000000000, -0.000000000000000000 ) ) ;
#194 = PRODUCT_DEFINITION_FORMATION_WITH_SPECIFIED_SOURCE ( 'ANY', '', #1335, .NOT_KNOWN. ) ;
#195 = VERTEX_POINT ( 'NONE', #1570 ) ;
#196 = ORIENTED_EDGE ( 'NONE', *, *, #2432, .T. ) ;
#197 = CARTESIAN_POINT ( 'NONE',  ( -7.619994990996017847, 12.08587093932537826, 18.40096039353565160 ) ) ;
#198 = AXIS2_PLACEMENT_3D ( 'NONE', #939, #3484, #1720 ) ;
#199 = UNCERTAINTY_MEASURE_WITH_UNIT (LENGTH_MEASURE( 1.000000000000000082E-05 ), #312, 'distance_accuracy_value', 'NONE');
#200 = ORIENTED_EDGE ( 'NONE', *, *, #995, .F. ) ;
#201 = CARTESIAN_POINT ( 'NONE',  ( -7.619992765438047044, -6.393402013451325416, 31.86762445358908735 ) ) ;
#202 = CARTESIAN_POINT ( 'NONE',  ( 6.586250505521797471, -12.25345428146915161, 6.586250505521797471 ) ) ;
#203 = CYLINDRICAL_SURFACE ( 'NONE', #1154, 7.147499999999999076 ) ;
#204 = CARTESIAN_POINT ( 'NONE',  ( 12.58215065716882819, 6.772263696356577434, 34.69848916189055643 ) ) ;
#205 = DIRECTION ( 'NONE',  ( 0.000000000000000000, 0.000000000000000000, -1.000000000000000000 ) ) ;
#206 = PLANE ( 'NONE',  #651 ) ;
#207 = AXIS2_PLACEMENT_3D ( 'NONE', #2433, #3594, #1816 ) ;
#208 = CARTESIAN_POINT ( 'NONE',  ( -14.12120247390863881, -2.178204474482083874, 29.02795621720992614 ) ) ;
#209 = VERTEX_POINT ( 'NONE', #2989 ) ;
#210 = CARTESIAN_POINT ( 'NONE',  ( 2.316727177394500794E-17, 0.000000000000000000, 1.587499999999999467 ) ) ;
#211 = EDGE_LOOP ( 'NONE', ( #1277, #2429, #378, #3663, #2254 ) ) ;
#212 = LINE ( 'NONE', #3385, #3482 ) ;
#213 = AXIS2_PLACEMENT_3D ( 'NONE', #1164, #1885, #2858 ) ;
#214 = ORIENTED_EDGE ( 'NONE', *, *, #499, .T. ) ;
#215 = DIRECTION ( 'NONE',  ( -1.000000000000000000, 8.673617379884035472E-16, -8.673617379884035472E-16 ) ) ;
#216 = AXIS2_PLACEMENT_3D ( 'NONE', #2791, #3106, #2092 ) ;
#217 = DIRECTION ( 'NONE',  ( 1.000000000000000000, 0.000000000000000000, 0.000000000000000000 ) ) ;
#218 = ORIENTED_EDGE ( 'NONE', *, *, #2621, .T. ) ;
#219 = ORIENTED_EDGE ( 'NONE', *, *, #1152, .T. ) ;
#220 = CARTESIAN_POINT ( 'NONE',  ( 18.74250723456195189, 0.004097986548670510577, 31.86762445358909446 ) ) ;
#221 = AXIS2_PLACEMENT_3D ( 'NONE', #1438, #2596, #3615 ) ;
#222 = ORIENTED_EDGE ( 'NONE', *, *, #2560, .T. ) ;
#223 = SPHERICAL_SURFACE ( 'NONE', #1597, 0.5000000000000000000 ) ;
#224 = CARTESIAN_POINT ( 'NONE',  ( -13.60391200005281753, -4.370503985835838101, 38.02622764783903619 ) ) ;
#225 = LINE ( 'NONE', #1603, #3538 ) ;
#226 = PRESENTATION_STYLE_ASSIGNMENT (( #1341 ) ) ;
#227 = CARTESIAN_POINT ( 'NONE',  ( -13.83332089671217169, -3.569652013451326322, 31.86762445358909446 ) ) ;
#228 = ORIENTED_EDGE ( 'NONE', *, *, #1349, .T. ) ;
#229 = LINE ( 'NONE', #603, #348 ) ;
#230 = VERTEX_POINT ( 'NONE', #2325 ) ;
#231 = CARTESIAN_POINT ( 'NONE',  ( 13.83333536583607959, 3.577847986548670978, 31.86762445358909446 ) ) ;
#232 = AXIS2_PLACEMENT_3D ( 'NONE', #4351, #46, #1908 ) ;
#233 = EDGE_CURVE ( 'NONE', #4049, #680, #4434, .T. ) ;
#234 = B_SPLINE_CURVE_WITH_KNOTS ( 'NONE', 3,
 ( #3727, #507, #4132, #3380, #204, #4464, #1951, #2335, #1251, #1299, #2666, #4107, #885, #2310, #3778, #1654, #3071, #4513, #2716, #4157, #2353, #3798, #2021, #3520 ),
 .UNSPECIFIED., .F., .F.,
 ( 4, 2, 2, 2, 2, 2, 2, 2, 2, 2, 2, 4 ),
 ( 0.000000000000000000, 0.001420218485702516619, 0.002840436971405033238, 0.004260655457107550073, 0.004970764699958816514, 0.005680873942810082955, 0.006390983185661350263, 0.007101092428512616704, 0.008521310914215162596, 0.009231420157066438578, 0.009941529399917716295, 0.01136174788562026999 ),
 .UNSPECIFIED. ) ;
#235 = ORIENTED_EDGE ( 'NONE', *, *, #3251, .F. ) ;
#236 = CIRCLE ( 'NONE', #4105, 7.147499999999999076 ) ;
#237 = DIRECTION ( 'NONE',  ( 0.000000000000000000, 0.000000000000000000, -1.000000000000000000 ) ) ;
#238 = PRODUCT_DEFINITION_SHAPE ( 'NONE', 'NONE',  #4651 ) ;
#239 = DIRECTION ( 'NONE',  ( 1.000000000000000000, 1.076498916035107621E-16, -0.000000000000000000 ) ) ;
#240 = AXIS2_PLACEMENT_3D ( 'NONE', #4426, #2657, #1612 ) ;
#241 = ORIENTED_EDGE ( 'NONE', *, *, #1369, .F. ) ;
#242 = ORIENTED_EDGE ( 'NONE', *, *, #4335, .T. ) ;
#243 = AXIS2_PLACEMENT_3D ( 'NONE', #3248, #4018, #4329 ) ;
#244 = PRESENTATION_STYLE_ASSIGNMENT (( #4572 ) ) ;
#245 = VERTEX_POINT ( 'NONE', #3401 ) ;
#246 = FACE_OUTER_BOUND ( 'NONE', #1430, .T. ) ;
#247 = CARTESIAN_POINT ( 'NONE',  ( 14.28750500900398279, 8.320472145953950175E-07, 35.93971039353566965 ) ) ;
#248 = CARTESIAN_POINT ( 'NONE',  ( -13.92229192741629262, -3.211036282058272739, 33.95194610545058822 ) ) ;
#249 = CARTESIAN_POINT ( 'NONE',  ( 2.540000505521796015, -3.039999999999999147, 17.78000050552179445 ) ) ;
#250 = FACE_OUTER_BOUND ( 'NONE', #4509, .T. ) ;
#251 = EDGE_CURVE ( 'NONE', #4208, #3225, #2015, .T. ) ;
#252 = CARTESIAN_POINT ( 'NONE',  ( -3.152215195724335395, -3.565902013451327068, -10.04237554641092345 ) ) ;
#253 = CYLINDRICAL_SURFACE ( 'NONE', #2742, 3.573749999999999538 ) ;
#254 = VERTEX_POINT ( 'NONE', #4484 ) ;
#255 = CARTESIAN_POINT ( 'NONE',  ( -6.869992765438047932, -6.393402013451324528, 17.90262445358908039 ) ) ;
#256 = AXIS2_PLACEMENT_3D ( 'NONE', #4355, #1062, #678 ) ;
#257 = ORIENTED_EDGE ( 'NONE', *, *, #1303, .F. ) ;
#258 = LINE ( 'NONE', #3153, #4263 ) ;
#259 = EDGE_CURVE ( 'NONE', #359, #3792, #1269, .T. ) ;
#260 = EDGE_CURVE ( 'NONE', #1840, #560, #2604, .T. ) ;
#261 = FACE_OUTER_BOUND ( 'NONE', #3718, .T. ) ;
#262 = ORIENTED_EDGE ( 'NONE', *, *, #4295, .T. ) ;
#263 = EDGE_CURVE ( 'NONE', #1498, #728, #3212, .T. ) ;
#264 = EDGE_LOOP ( 'NONE', ( #3177, #543, #4448, #1020 ) ) ;
#265 = EDGE_CURVE ( 'NONE', #2363, #680, #2439, .T. ) ;
#266 = DIRECTION ( 'NONE',  ( 8.673617379884035472E-17, 1.000000000000000000, -0.000000000000000000 ) ) ;
#267 = ORIENTED_EDGE ( 'NONE', *, *, #1508, .F. ) ;
#268 = LINE ( 'NONE', #2393, #3299 ) ;
#269 = CARTESIAN_POINT ( 'NONE',  ( -14.17582296520950713, -1.793657354674257354, 35.46585984560420712 ) ) ;
#270 = CARTESIAN_POINT ( 'NONE',  ( 13.83079035606262508, -3.606001054908336112, 38.55461960823348022 ) ) ;
#271 = AXIS2_PLACEMENT_3D ( 'NONE', #3619, #4325, #2577 ) ;
#272 = CARTESIAN_POINT ( 'NONE',  ( -14.28749499099602005, 8.320472128100571937E-07, 28.79221039353566880 ) ) ;
#273 = DIRECTION ( 'NONE',  ( 0.000000000000000000, 0.000000000000000000, 1.000000000000000000 ) ) ;
#274 = FACE_OUTER_BOUND ( 'NONE', #558, .T. ) ;
#275 = MANIFOLD_SOLID_BREP ( 'Ölçek1', #1022 ) ;
#276 = DIRECTION ( 'NONE',  ( -1.000000000000000000, 1.076498916035107744E-16, 0.000000000000000000 ) ) ;
#277 = ORIENTED_EDGE ( 'NONE', *, *, #2701, .T. ) ;
#278 = CARTESIAN_POINT ( 'NONE',  ( 13.23919276269517020, -5.370076350862035497, 36.58546145169297859 ) ) ;
#279 = DIRECTION ( 'NONE',  ( -1.000000000000000000, 0.000000000000000000, 0.000000000000000000 ) ) ;
#280 = EDGE_CURVE ( 'NONE', #719, #1143, #3487, .T. ) ;
#281 = ORIENTED_EDGE ( 'NONE', *, *, #2560, .F. ) ;
#282 = ORIENTED_EDGE ( 'NONE', *, *, #177, .F. ) ;
#283 = AXIS2_PLACEMENT_3D ( 'NONE', #969, #1010, #610 ) ;
#284 = CARTESIAN_POINT ( 'NONE',  ( -3.750000000000000000, 3.750000000000000000, 18.74999999999999645 ) ) ;
#285 = VECTOR ( 'NONE', #339, 1000.000000000000000 ) ;
#286 = EDGE_CURVE ( 'NONE', #1844, #313, #1692, .T. ) ;
#287 = ORIENTED_EDGE ( 'NONE', *, *, #1174, .F. ) ;
#288 = DIRECTION ( 'NONE',  ( 0.000000000000000000, 0.000000000000000000, 1.000000000000000000 ) ) ;
#289 = DIRECTION ( 'NONE',  ( 1.000000000000000000, -0.000000000000000000, -0.000000000000000000 ) ) ;
#290 =( REPRESENTATION_RELATIONSHIP ('NONE','NONE', #4401, #1824 ) REPRESENTATION_RELATIONSHIP_WITH_TRANSFORMATION ( #3328 )SHAPE_REPRESENTATION_RELATIONSHIP( ) );
#291 = CARTESIAN_POINT ( 'NONE',  ( -12.13298098450732354, 7.549547314929181852, 17.23390984512910507 ) ) ;
#292 = VECTOR ( 'NONE', #482, 1000.000000000000000 ) ;
#293 = CARTESIAN_POINT ( 'NONE',  ( 12.58716054243624249, -6.760358215630333234, 34.69836126359587070 ) ) ;
#294 = DIRECTION ( 'NONE',  ( -0.000000000000000000, 1.000000000000000000, 0.000000000000000000 ) ) ;
#295 =( GEOMETRIC_REPRESENTATION_CONTEXT ( 3 ) GLOBAL_UNCERTAINTY_ASSIGNED_CONTEXT ( ( #2687 ) ) GLOBAL_UNIT_ASSIGNED_CONTEXT ( ( #3953, #4645, #1803 ) ) REPRESENTATION_CONTEXT ( 'NONE', 'WORKASPACE' ) );
#296 = DIRECTION ( 'NONE',  ( 0.000000000000000000, -0.000000000000000000, -1.000000000000000000 ) ) ;
#297 = DIRECTION ( 'NONE',  ( 1.000000000000000000, -1.076498916035107621E-16, -0.000000000000000000 ) ) ;
#298 = CARTESIAN_POINT ( 'NONE',  ( -3.750000000000000888, -3.750000000000000000, 3.749999999999995559 ) ) ;
#299 = DIRECTION ( 'NONE',  ( 0.000000000000000000, 0.000000000000000000, 1.000000000000000000 ) ) ;
#300 = CARTESIAN_POINT ( 'NONE',  ( 12.37117936981252164, -7.143402013451325416, 17.90262445358908039 ) ) ;
#301 = VECTOR ( 'NONE', #694, 1000.000000000000000 ) ;
#302 = ORIENTED_EDGE ( 'NONE', *, *, #1589, .T. ) ;
#303 = EDGE_CURVE ( 'NONE', #1254, #359, #4238, .T. ) ;
#304 = LINE ( 'NONE', #2457, #806 ) ;
#305 = AXIS2_PLACEMENT_3D ( 'NONE', #1975, #3706, #3407 ) ;
#306 = CARTESIAN_POINT ( 'NONE',  ( 6.870007234561950504, -6.393402013451325416, 17.90262445358908039 ) ) ;
#307 = CIRCLE ( 'NONE', #4141, 0.5000000000000004441 ) ;
#308 = ORIENTED_EDGE ( 'NONE', *, *, #2151, .T. ) ;
#309 = AXIS2_PLACEMENT_3D ( 'NONE', #1170, #75, #1587 ) ;
#310 = ORIENTED_EDGE ( 'NONE', *, *, #1590, .T. ) ;
#311 = AXIS2_PLACEMENT_3D ( 'NONE', #4250, #3824, #4584 ) ;
#312 =( LENGTH_UNIT ( ) NAMED_UNIT ( * ) SI_UNIT ( .MILLI., .METRE. ) );
#313 = VERTEX_POINT ( 'NONE', #2097 ) ;
#314 = DIRECTION ( 'NONE',  ( 1.000000000000000000, 0.000000000000000000, 0.000000000000000000 ) ) ;
#315 = ORIENTED_EDGE ( 'NONE', *, *, #4091, .F. ) ;
#316 = CARTESIAN_POINT ( 'NONE',  ( -14.03269519519255759, 2.695605797375577151, 29.50494583009495742 ) ) ;
#317 = DIRECTION ( 'NONE',  ( 1.318389841742373392E-16, -1.000000000000000000, 0.000000000000000000 ) ) ;
#318 = CARTESIAN_POINT ( 'NONE',  ( -14.05880083816784598, -2.555479569424798036, 39.04506677964694461 ) ) ;
#319 = LINE ( 'NONE', #249, #4138 ) ;
#320 = CYLINDRICAL_SURFACE ( 'NONE', #2187, 0.5000000000000000000 ) ;
#321 = DIRECTION ( 'NONE',  ( 0.000000000000000000, 0.000000000000000000, 1.000000000000000000 ) ) ;
#322 = CARTESIAN_POINT ( 'NONE',  ( -13.92260781862683672, -3.209692932854570024, 30.77693904423523819 ) ) ;
#323 = ADVANCED_BREP_SHAPE_REPRESENTATION ( '', ( #3432, #4483 ), #3865 ) ;
#324 = APPLICATION_CONTEXT ( 'automotive_design' ) ;
#325 = DIRECTION ( 'NONE',  ( 0.000000000000000000, 0.000000000000000000, 1.000000000000000000 ) ) ;
#326 = CARTESIAN_POINT ( 'NONE',  ( 3.750000000000000888, -3.750000000000000000, 131.2499999999999716 ) ) ;
#327 = CARTESIAN_POINT ( 'NONE',  ( -8.369992765438045268, -7.893402013451320975, 17.15262445358908039 ) ) ;
#328 = ADVANCED_FACE ( 'NONE', ( #3115 ), #973, .F. ) ;
#329 = EDGE_CURVE ( 'NONE', #1870, #4530, #4549, .T. ) ;
#330 = ORIENTED_EDGE ( 'NONE', *, *, #3902, .T. ) ;
#331 = DIRECTION ( 'NONE',  ( 0.000000000000000000, -1.000000000000000000, 0.000000000000000000 ) ) ;
#332 = VECTOR ( 'NONE', #1088, 1000.000000000000000 ) ;
#333 = CARTESIAN_POINT ( 'NONE',  ( 14.28750000000000142, 1.746464731918909201E-15, 18.74999999999999645 ) ) ;
#334 = EDGE_LOOP ( 'NONE', ( #4411, #4153, #2795, #3553 ) ) ;
#335 = EDGE_LOOP ( 'NONE', ( #948, #1406 ) ) ;
#336 = ORIENTED_EDGE ( 'NONE', *, *, #4404, .T. ) ;
#337 = CARTESIAN_POINT ( 'NONE',  ( 12.35764254201991719, 7.171053272434127379, 18.18681329310062011 ) ) ;
#338 = VERTEX_POINT ( 'NONE', #2390 ) ;
#339 = DIRECTION ( 'NONE',  ( -1.000000000000000000, -0.000000000000000000, -0.000000000000000000 ) ) ;
#340 = CARTESIAN_POINT ( 'NONE',  ( 13.48444558334203691, 4.730385405907853169, 37.23438744284854351 ) ) ;
#341 = DIRECTION ( 'NONE',  ( 0.000000000000000000, -0.000000000000000000, 1.000000000000000000 ) ) ;
#342 = AXIS2_PLACEMENT_3D ( 'NONE', #6, #2515, #3188 ) ;
#343 = CARTESIAN_POINT ( 'NONE',  ( 6.586250505521797471, -10.16000000000000014, 17.78000050552179445 ) ) ;
#344 = EDGE_CURVE ( 'NONE', #4402, #4095, #478, .T. ) ;
#345 = CARTESIAN_POINT ( 'NONE',  ( 8.370007234561949616, 6.401597986548672736, 17.15262445358908039 ) ) ;
#346 = CARTESIAN_POINT ( 'NONE',  ( 8.370007234561949616, -6.393402013451325416, 17.15262445358908039 ) ) ;
#347 = DIRECTION ( 'NONE',  ( 1.000000000000000000, 0.000000000000000000, 0.000000000000000000 ) ) ;
#348 = VECTOR ( 'NONE', #1681, 1000.000000000000000 ) ;
#349 = CARTESIAN_POINT ( 'NONE',  ( 3.750005009003979595, 3.750000832047212906, 18.79096039353565217 ) ) ;
#350 = ORIENTED_EDGE ( 'NONE', *, *, #1980, .F. ) ;
#351 = CARTESIAN_POINT ( 'NONE',  ( 13.83333314027810701, 3.573750832047211112, 32.83350159718256123 ) ) ;
#352 = AXIS2_PLACEMENT_3D ( 'NONE', #3185, #4020, #314 ) ;
#353 = DIRECTION ( 'NONE',  ( -1.000000000000000000, 0.000000000000000000, 0.000000000000000000 ) ) ;
#354 = VECTOR ( 'NONE', #814, 1000.000000000000000 ) ;
#355 = EDGE_LOOP ( 'NONE', ( #267, #1778 ) ) ;
#356 = VERTEX_POINT ( 'NONE', #2750 ) ;
#357 = PRESENTATION_STYLE_ASSIGNMENT (( #1496 ) ) ;
#358 = AXIS2_PLACEMENT_3D ( 'NONE', #3782, #2976, #2651 ) ;
#359 = VERTEX_POINT ( 'NONE', #284 ) ;
#360 = CARTESIAN_POINT ( 'NONE',  ( 12.27079714706309055, 7.318983740777395219, 17.91363472736960816 ) ) ;
#361 = EDGE_CURVE ( 'NONE', #3625, #1713, #3063, .T. ) ;
#362 = CARTESIAN_POINT ( 'NONE',  ( 2.540000505521796015, -10.16000000000000014, 10.16000050552179701 ) ) ;
#363 = MANIFOLD_SOLID_BREP ( 'Ölçek1', #3046 ) ;
#364 = APPLICATION_PROTOCOL_DEFINITION ( 'draft international standard', 'automotive_design', 1998, #1357 ) ;
#365 = EDGE_CURVE ( 'NONE', #4505, #675, #3257, .T. ) ;
#366 = CARTESIAN_POINT ( 'NONE',  ( 8.370007234561949616, 6.401597986548672736, 3.292624453589077405 ) ) ;
#367 = CARTESIAN_POINT ( 'NONE',  ( 14.99250723456195544, 7.151597986548670072, 3.292624453589077405 ) ) ;
#368 = FACE_OUTER_BOUND ( 'NONE', #29, .T. ) ;
#369 = CARTESIAN_POINT ( 'NONE',  ( -8.369992765438045268, -6.393402013451324528, 17.15262445358908039 ) ) ;
#370 = CARTESIAN_POINT ( 'NONE',  ( -14.12109987650483056, -2.178937149005899521, 34.70680459945198493 ) ) ;
#371 = DIRECTION ( 'NONE',  ( -1.000000000000000000, 1.076498916035107621E-16, 0.000000000000000000 ) ) ;
#372 = AXIS2_PLACEMENT_3D ( 'NONE', #860, #2622, #4439 ) ;
#373 = ORIENTED_EDGE ( 'NONE', *, *, #3936, .F. ) ;
#374 = DIRECTION ( 'NONE',  ( 0.000000000000000000, -1.000000000000000000, 0.000000000000000000 ) ) ;
#375 = EDGE_CURVE ( 'NONE', #2669, #3403, #4284, .T. ) ;
#376 = FACE_BOUND ( 'NONE', #1894, .T. ) ;
#377 = SPHERICAL_SURFACE ( 'NONE', #256, 0.5000000000000000000 ) ;
#378 = ORIENTED_EDGE ( 'NONE', *, *, #2676, .T. ) ;
#379 = ORIENTED_EDGE ( 'NONE', *, *, #3374, .F. ) ;
#380 = CARTESIAN_POINT ( 'NONE',  ( -14.28749276543804392, 0.4849387513329158628, 39.01512445358908820 ) ) ;
#381 = EDGE_CURVE ( 'NONE', #1044, #2857, #1512, .T. ) ;
#382 = EDGE_LOOP ( 'NONE', ( #2847, #4617 ) ) ;
#383 = ORIENTED_EDGE ( 'NONE', *, *, #467, .F. ) ;
#384 = CIRCLE ( 'NONE', #756, 14.28750000000000142 ) ;
#385 = CARTESIAN_POINT ( 'NONE',  ( -6.869992765438046156, 0.004097986548673267920, 17.15262445358908039 ) ) ;
#386 = VECTOR ( 'NONE', #4108, 1000.000000000000000 ) ;
#387 = LINE ( 'NONE', #3242, #464 ) ;
#388 = CIRCLE ( 'NONE', #2641, 0.5000000000000004441 ) ;
#389 = FACE_OUTER_BOUND ( 'NONE', #4126, .T. ) ;
#390 = DIRECTION ( 'NONE',  ( 1.000000000000000000, 0.000000000000000000, 0.000000000000000000 ) ) ;
#391 = MANIFOLD_SOLID_BREP ( 'Radyus1', #3647 ) ;
#392 = CARTESIAN_POINT ( 'NONE',  ( -14.03259092081030701, -2.687846779405278053, 34.22958848126887688 ) ) ;
#393 = FILL_AREA_STYLE ('',( #17 ) ) ;
#394 = DIRECTION ( 'NONE',  ( 1.000000000000000000, 0.000000000000000000, 0.000000000000000000 ) ) ;
#395 = EDGE_CURVE ( 'NONE', #1844, #3471, #2461, .T. ) ;
#396 = ORIENTED_EDGE ( 'NONE', *, *, #2346, .T. ) ;
#397 = CARTESIAN_POINT ( 'NONE',  ( 14.00306134798043800, 2.839839263610262954, 34.54803640670024123 ) ) ;
#398 = CARTESIAN_POINT ( 'NONE',  ( -14.26328196213224508, -0.9495361258265833104, 38.96707689327597279 ) ) ;
#399 = B_SPLINE_CURVE_WITH_KNOTS ( 'NONE', 3,
 ( #440, #4305, #2931, #3316, #4379, #1188, #791, #2184, #3622, #1866, #3997, #1165, #3948, #1560, #3341, #2580, #2252, #1140, #2953, #3598, #2556, #398, #4399, #768 ),
 .UNSPECIFIED., .F., .F.,
 ( 4, 2, 2, 2, 2, 2, 2, 2, 2, 2, 2, 4 ),
 ( -0.01136693575711654296, -0.009946068787476983544, -0.008525201817837424131, -0.007104334848197864719, -0.006393901363378076338, -0.005683467878558287091, -0.004973034393738498711, -0.004262600908918711198, -0.002841733939279146581, -0.002131300454459359936, -0.001420866969639575025, -1.734723475976807094E-18 ),
 .UNSPECIFIED. ) ;
#400 = CARTESIAN_POINT ( 'NONE',  ( 2.316727177394501718E-17, 0.000000000000000000, 33.33750000000000568 ) ) ;
#401 = EDGE_CURVE ( 'NONE', #2368, #1254, #2888, .T. ) ;
#402 = ORIENTED_EDGE ( 'NONE', *, *, #4582, .T. ) ;
#403 = EDGE_LOOP ( 'NONE', ( #3744, #2182 ) ) ;
#404 = EDGE_CURVE ( 'NONE', #1899, #4499, #3693, .T. ) ;
#405 = EDGE_LOOP ( 'NONE', ( #1015, #2600, #235, #1549 ) ) ;
#406 = EDGE_CURVE ( 'NONE', #2052, #4636, #1215, .T. ) ;
#407 = CARTESIAN_POINT ( 'NONE',  ( 7.234561953626996335E-06, 0.004097986548672528061, 17.15262445358908039 ) ) ;
#408 = DIRECTION ( 'NONE',  ( 3.825249650243476815E-17, -1.437806642091473824E-17, -1.000000000000000000 ) ) ;
#409 = CARTESIAN_POINT ( 'NONE',  ( -8.369994990996016071, 6.397500832047212427, 18.40096039353565160 ) ) ;
#410 = PLANE ( 'NONE',  #1786 ) ;
#411 = CARTESIAN_POINT ( 'NONE',  ( -13.87970419316790682, -3.390420155928260293, 31.21176438016646770 ) ) ;
#412 = CARTESIAN_POINT ( 'NONE',  ( 3.750000000000000888, -3.750000000000000000, 131.2499999999999716 ) ) ;
#413 = DIRECTION ( 'NONE',  ( -1.000000000000000000, -0.000000000000000000, -0.000000000000000000 ) ) ;
#414 = CARTESIAN_POINT ( 'NONE',  ( 14.25924652348691524, -0.9230119033506298809, 35.32694493162775018 ) ) ;
#415 = CARTESIAN_POINT ( 'NONE',  ( 12.30738649273683372, -7.256959721446875733, 17.99723211794410460 ) ) ;
#416 = PRODUCT_DEFINITION_FORMATION_WITH_SPECIFIED_SOURCE ( 'ANY', '', #1031, .NOT_KNOWN. ) ;
#417 = ORIENTED_EDGE ( 'NONE', *, *, #13, .T. ) ;
#418 = DIRECTION ( 'NONE',  ( -1.000000000000000000, -1.076498916035107621E-16, 0.000000000000000000 ) ) ;
#419 = AXIS2_PLACEMENT_3D ( 'NONE', #582, #2380, #2739 ) ;
#420 = DIRECTION ( 'NONE',  ( 1.000000000000000000, 0.000000000000000000, 0.000000000000000000 ) ) ;
#421 = VERTEX_POINT ( 'NONE', #798 ) ;
#422 = CIRCLE ( 'NONE', #2440, 0.7500000000000006661 ) ;
#423 = CARTESIAN_POINT ( 'NONE',  ( 17.78000050552179445, -10.16000000000000014, 10.16000050552179701 ) ) ;
#424 = EDGE_CURVE ( 'NONE', #356, #3559, #902, .T. ) ;
#425 = ORIENTED_EDGE ( 'NONE', *, *, #601, .F. ) ;
#426 = ORIENTED_EDGE ( 'NONE', *, *, #1490, .F. ) ;
#427 = DIRECTION ( 'NONE',  ( 1.000000000000000000, -0.000000000000000000, -0.000000000000000000 ) ) ;
#428 = CARTESIAN_POINT ( 'NONE',  ( 14.28155663460688984, 0.4719428512367060402, 28.81578682141157444 ) ) ;
#429 = EDGE_CURVE ( 'NONE', #4385, #3952, #3669, .T. ) ;
#430 = CARTESIAN_POINT ( 'NONE',  ( 11.90639837545767321, 7.901597986548669184, 17.15262445358908039 ) ) ;
#431 = CIRCLE ( 'NONE', #3662, 0.7500000000000006661 ) ;
#432 = CARTESIAN_POINT ( 'NONE',  ( 6.586250505521797471, -8.066545718530848674, 6.586250505521797471 ) ) ;
#433 = DIRECTION ( 'NONE',  ( 9.517981353260378315E-33, 8.841607930564763213E-17, -1.000000000000000000 ) ) ;
#434 = CARTESIAN_POINT ( 'NONE',  ( 14.99250500900398109, 7.147500832047209762, 32.36596039353565857 ) ) ;
#435 = CARTESIAN_POINT ( 'NONE',  ( -14.28749276543804747, -0.2329318086950452060, 35.44137445358909133 ) ) ;
#436 = CIRCLE ( 'NONE', #2760, 0.7500000000000006661 ) ;
#437 = CARTESIAN_POINT ( 'NONE',  ( -9.549434556529077899E-17, -3.249382362871961689E-18, 18.74999999999999645 ) ) ;
#438 = ORIENTED_EDGE ( 'NONE', *, *, #1098, .F. ) ;
#439 = DIRECTION ( 'NONE',  ( 0.000000000000000000, 0.000000000000000000, 1.000000000000000000 ) ) ;
#440 = CARTESIAN_POINT ( 'NONE',  ( -12.37116490068861197, -7.143402013451323640, 31.86762445358908735 ) ) ;
#441 = AXIS2_PLACEMENT_3D ( 'NONE', #2692, #532, #1950 ) ;
#442 = DIRECTION ( 'NONE',  ( -1.000000000000000000, 1.076498916035107621E-16, 0.000000000000000000 ) ) ;
#443 = EDGE_LOOP ( 'NONE', ( #2753, #3813, #2295, #1561, #4044 ) ) ;
#444 = DIRECTION ( 'NONE',  ( -1.707404996040164265E-16, 1.000000000000000000, 0.000000000000000000 ) ) ;
#445 = CARTESIAN_POINT ( 'NONE',  ( 3.749999999999999556, -3.750000000000000888, 3.749999999999995559 ) ) ;
#446 = DIRECTION ( 'NONE',  ( 0.000000000000000000, 1.000000000000000000, 0.000000000000000000 ) ) ;
#447 = LINE ( 'NONE', #3345, #4260 ) ;
#448 = EDGE_CURVE ( 'NONE', #4520, #4090, #3716, .T. ) ;
#449 = ORIENTED_EDGE ( 'NONE', *, *, #526, .F. ) ;
#450 = CARTESIAN_POINT ( 'NONE',  ( -13.48424419627515292, 4.726824056057109757, 37.73224719609674338 ) ) ;
#451 = AXIS2_PLACEMENT_3D ( 'NONE', #1765, #2065, #670 ) ;
#452 = CARTESIAN_POINT ( 'NONE',  ( -13.23918051912923666, 5.374175169457920731, 37.08379739163955691 ) ) ;
#453 = CARTESIAN_POINT ( 'NONE',  ( -12.35763029845398364, -7.166954453838238592, 17.68847735315405245 ) ) ;
#454 = ORIENTED_EDGE ( 'NONE', *, *, #3428, .F. ) ;
#455 = FACE_OUTER_BOUND ( 'NONE', #868, .T. ) ;
#456 = EDGE_CURVE ( 'NONE', #1954, #992, #4200, .T. ) ;
#457 =( LENGTH_UNIT ( ) NAMED_UNIT ( * ) SI_UNIT ( .MILLI., .METRE. ) );
#458 =( NAMED_UNIT ( * ) SI_UNIT ( $, .STERADIAN. ) SOLID_ANGLE_UNIT ( ) );
#459 = CARTESIAN_POINT ( 'NONE',  ( -12.37116490068860841, 7.151597986548674513, 17.79434398117761518 ) ) ;
#460 = VECTOR ( 'NONE', #2087, 1000.000000000000000 ) ;
#461 = CARTESIAN_POINT ( 'NONE',  ( 14.99250723456195189, 0.004097986548670913901, 31.86762445358908735 ) ) ;
#462 = CARTESIAN_POINT ( 'NONE',  ( -7.619992765438038163, 7.901597986548672736, 17.15262445358908039 ) ) ;
#463 = CARTESIAN_POINT ( 'NONE',  ( -7.619994990996021400, -6.397499167952786614, 32.36596039353565857 ) ) ;
#464 = VECTOR ( 'NONE', #3232, 1000.000000000000000 ) ;
#465 = ORIENTED_EDGE ( 'NONE', *, *, #365, .T. ) ;
#466 = CARTESIAN_POINT ( 'NONE',  ( 3.750005009003979595, -3.749999167952787538, 18.79096039353565217 ) ) ;
#467 = EDGE_CURVE ( 'NONE', #4067, #3625, #2172, .T. ) ;
#468 = VECTOR ( 'NONE', #4539, 1000.000000000000000 ) ;
#469 = CARTESIAN_POINT ( 'NONE',  ( 3.750000000000000000, 3.750000000000000000, 131.2499999999999716 ) ) ;
#470 = ADVANCED_FACE ( 'NONE', ( #3301 ), #3368, .F. ) ;
#471 = CYLINDRICAL_SURFACE ( 'NONE', #3708, 0.7500000000000006661 ) ;
#472 = ORIENTED_EDGE ( 'NONE', *, *, #741, .F. ) ;
#473 = CARTESIAN_POINT ( 'NONE',  ( 14.24236788465317538, -1.151086274564850909, 28.47772737627938611 ) ) ;
#474 = APPLICATION_CONTEXT ( 'automotive_design' ) ;
#475 = DIRECTION ( 'NONE',  ( 0.000000000000000000, 1.000000000000000000, 0.000000000000000000 ) ) ;
#476 = ORIENTED_EDGE ( 'NONE', *, *, #865, .F. ) ;
#477 = EDGE_LOOP ( 'NONE', ( #2137, #523 ) ) ;
#478 =( BOUNDED_CURVE ( )  B_SPLINE_CURVE ( 3, ( #2081, #2730, #3495, #2370 ),
 .UNSPECIFIED., .F., .T. ) 
 B_SPLINE_CURVE_WITH_KNOTS ( ( 4, 4 ),
 ( 0.000000000000000000, 1.570796326794896558 ),
 .UNSPECIFIED. ) 
 CURVE ( )  GEOMETRIC_REPRESENTATION_ITEM ( )  RATIONAL_B_SPLINE_CURVE ( ( 1.000000000000000000, 0.8047378541243649375, 0.8047378541243649375, 1.000000000000000000 ) ) 
 REPRESENTATION_ITEM ( '' )  );
#479 = CARTESIAN_POINT ( 'NONE',  ( 7.620007234561953169, -3.569652013451328099, 31.86762445358909446 ) ) ;
#480 = ORIENTED_EDGE ( 'NONE', *, *, #3902, .F. ) ;
#481 = FACE_OUTER_BOUND ( 'NONE', #1065, .T. ) ;
#482 = DIRECTION ( 'NONE',  ( -0.000000000000000000, -0.000000000000000000, 1.000000000000000000 ) ) ;
#483 = CYLINDRICAL_SURFACE ( 'NONE', #829, 3.573749999999998650 ) ;
#484 = DIRECTION ( 'NONE',  ( -1.076498916035107621E-16, -1.000000000000000000, 0.000000000000000000 ) ) ;
#485 = ADVANCED_FACE ( 'NONE', ( #1868 ), #2298, .F. ) ;
#486 = ORIENTED_EDGE ( 'NONE', *, *, #120, .F. ) ;
#487 = CARTESIAN_POINT ( 'NONE',  ( -12.37116712624658810, -7.147499167952783061, 17.65096039353565160 ) ) ;
#488 = PLANE ( 'NONE',  #2053 ) ;
#489 = ORIENTED_EDGE ( 'NONE', *, *, #4501, .T. ) ;
#490 = DIRECTION ( 'NONE',  ( 0.000000000000000000, 0.000000000000000000, -1.000000000000000000 ) ) ;
#491 = AXIS2_PLACEMENT_3D ( 'NONE', #3819, #1338, #2755 ) ;
#492 = DIRECTION ( 'NONE',  ( -1.000000000000000000, -0.000000000000000000, -0.000000000000000000 ) ) ;
#493 = CARTESIAN_POINT ( 'NONE',  ( 13.94789458910929980, 3.103566891827359786, 33.66190161997707975 ) ) ;
#494 = ORIENTED_EDGE ( 'NONE', *, *, #3566, .F. ) ;
#495 = ORIENTED_EDGE ( 'NONE', *, *, #520, .F. ) ;
#496 = ITEM_DEFINED_TRANSFORMATION ( 'NONE', 'NONE', #342,  #4483 ) ;
#497 = CARTESIAN_POINT ( 'NONE',  ( 13.86272949647482200, 3.458292335070031864, 31.43485104414858711 ) ) ;
#498 = LINE ( 'NONE', #2965, #2859 ) ;
#499 = EDGE_CURVE ( 'NONE', #1954, #3048, #2558, .T. ) ;
#500 = PRODUCT_DEFINITION ( 'UNKNOWN', '', #3721, #1613 ) ;
#501 = VERTEX_POINT ( 'NONE', #2658 ) ;
#502 = CIRCLE ( 'NONE', #4412, 0.7500000000000006661 ) ;
#503 = CARTESIAN_POINT ( 'NONE',  ( -12.37116490068859775, 7.151597986548673624, 31.86762445358908735 ) ) ;
#504 =( NAMED_UNIT ( * ) PLANE_ANGLE_UNIT ( ) SI_UNIT ( $, .RADIAN. ) );
#505 = EDGE_CURVE ( 'NONE', #3774, #4040, #537, .T. ) ;
#506 = DIRECTION ( 'NONE',  ( -1.000000000000000000, 1.076498916035107744E-16, 0.000000000000000000 ) ) ;
#507 = CARTESIAN_POINT ( 'NONE',  ( 12.37117714425454551, 7.147500832047209762, 32.84697568125973532 ) ) ;
#508 = LINE ( 'NONE', #934, #679 ) ;
#509 = CARTESIAN_POINT ( 'NONE',  ( 8.370007234561949616, -6.393402013451325416, 17.90262445358908039 ) ) ;
#510 = CIRCLE ( 'NONE', #568, 3.573749999999998650 ) ;
#511 = ORIENTED_EDGE ( 'NONE', *, *, #2401, .F. ) ;
#512 = CARTESIAN_POINT ( 'NONE',  ( 6.870005009003979701, 8.320472135496153183E-07, 17.65096039353565160 ) ) ;
#513 = CARTESIAN_POINT ( 'NONE',  ( 14.00286465610359699, 2.844890123102346013, 29.68689173443506490 ) ) ;
#514 = TOROIDAL_SURFACE ( 'NONE', #1725, 6.397499999999999964, 0.7500000000000000000 ) ;
#515 = ORIENTED_EDGE ( 'NONE', *, *, #3366, .F. ) ;
#516 = CARTESIAN_POINT ( 'NONE',  ( 14.03294702938207017, -2.686088116544980586, 29.50362573057097748 ) ) ;
#517 = CARTESIAN_POINT ( 'NONE',  ( -14.00302961127090029, 2.839984366820609729, 34.54801793703359891 ) ) ;
#518 = PRODUCT_DEFINITION_CONTEXT ( 'detailed design', #2244, 'design' ) ;
#519 = DIRECTION ( 'NONE',  ( 0.000000000000000000, 0.000000000000000000, -1.000000000000000000 ) ) ;
#520 = EDGE_CURVE ( 'NONE', #2793, #952, #4405, .T. ) ;
#521 = CARTESIAN_POINT ( 'NONE',  ( 13.83333314027810701, 3.573750832047210668, 32.36596039353566567 ) ) ;
#522 = VECTOR ( 'NONE', #2236, 1000.000000000000000 ) ;
#523 = ORIENTED_EDGE ( 'NONE', *, *, #3458, .F. ) ;
#524 = ORIENTED_EDGE ( 'NONE', *, *, #4084, .T. ) ;
#525 = CARTESIAN_POINT ( 'NONE',  ( 3.750005009003979595, -3.749999167952787538, 3.790960393535649064 ) ) ;
#526 = EDGE_CURVE ( 'NONE', #501, #1254, #2610, .T. ) ;
#527 = EDGE_CURVE ( 'NONE', #2126, #1592, #1914, .T. ) ;
#528 = AXIS2_PLACEMENT_3D ( 'NONE', #3551, #299, #1006 ) ;
#529 = ORIENTED_EDGE ( 'NONE', *, *, #4352, .T. ) ;
#530 = DIRECTION ( 'NONE',  ( 1.000000000000000000, 0.000000000000000000, 0.000000000000000000 ) ) ;
#531 = DIRECTION ( 'NONE',  ( 0.000000000000000000, 0.000000000000000000, 1.000000000000000000 ) ) ;
#532 = DIRECTION ( 'NONE',  ( 0.000000000000000000, 0.000000000000000000, 1.000000000000000000 ) ) ;
#533 = AXIS2_PLACEMENT_3D ( 'NONE', #3219, #2856, #2427 ) ;
#534 = FACE_OUTER_BOUND ( 'NONE', #2535, .T. ) ;
#535 = DIRECTION ( 'NONE',  ( 0.000000000000000000, 0.000000000000000000, 1.000000000000000000 ) ) ;
#536 = CARTESIAN_POINT ( 'NONE',  ( 2.540000505521796015, -2.539999999999999591, 17.28000050552179445 ) ) ;
#537 = CIRCLE ( 'NONE', #309, 0.5000000000000000000 ) ;
#538 = ORIENTED_EDGE ( 'NONE', *, *, #3424, .F. ) ;
#539 = CARTESIAN_POINT ( 'NONE',  ( 12.37117936981251809, -7.143402013451325416, 17.79434398117761518 ) ) ;
#540 = STYLED_ITEM ( 'NONE', ( #3656 ), #3432 ) ;
#541 = LINE ( 'NONE', #2628, #2266 ) ;
#542 = EDGE_CURVE ( 'NONE', #3954, #2747, #3742, .T. ) ;
#543 = ORIENTED_EDGE ( 'NONE', *, *, #3769, .F. ) ;
#544 = CARTESIAN_POINT ( 'NONE',  ( -13.92217922470506153, 3.211518876436516567, 33.95088485475975659 ) ) ;
#545 = CARTESIAN_POINT ( 'NONE',  ( -7.619994990996011630, 7.897500832047212427, 17.65096039353565160 ) ) ;
#546 = CARTESIAN_POINT ( 'NONE',  ( 14.24247936672400172, 1.158380674401813248, 35.25801904860673375 ) ) ;
#547 = EDGE_CURVE ( 'NONE', #4090, #3312, #3392, .T. ) ;
#548 = ORIENTED_EDGE ( 'NONE', *, *, #2840, .T. ) ;
#549 = ORIENTED_EDGE ( 'NONE', *, *, #3023, .T. ) ;
#550 = CARTESIAN_POINT ( 'NONE',  ( 13.83333314027810701, 3.573750832047211112, 32.13223144433574419 ) ) ;
#551 = ORIENTED_EDGE ( 'NONE', *, *, #1276, .F. ) ;
#552 = CIRCLE ( 'NONE', #2205, 0.7500000000000006661 ) ;
#553 = CARTESIAN_POINT ( 'NONE',  ( 5.708183634273623852, -3.565902013451327068, -1.469875546410923661 ) ) ;
#554 = DIRECTION ( 'NONE',  ( 0.000000000000000000, 0.000000000000000000, 1.000000000000000000 ) ) ;
#555 = CARTESIAN_POINT ( 'NONE',  ( 3.573749999999998650, 4.376581498452851814E-16, 33.33750000000000568 ) ) ;
#556 = CARTESIAN_POINT ( 'NONE',  ( -14.12134633028087372, 2.185469490339439602, 34.70800415505340908 ) ) ;
#557 = CARTESIAN_POINT ( 'NONE',  ( 12.37117936981252164, -7.143402013451325416, 17.90262445358908039 ) ) ;
#558 = EDGE_LOOP ( 'NONE', ( #3534, #1921, #2456, #145 ) ) ;
#559 = LINE ( 'NONE', #4518, #4646 ) ;
#560 = VERTEX_POINT ( 'NONE', #3031 ) ;
#561 = CARTESIAN_POINT ( 'NONE',  ( 7.620005009003980589, -6.397499167952787502, 32.36596039353565857 ) ) ;
#562 = PRODUCT_DEFINITION_SHAPE ( 'NONE', 'NONE',  #4655 ) ;
#563 = VERTEX_POINT ( 'NONE', #4475 ) ;
#564 = FACE_BOUND ( 'NONE', #2564, .T. ) ;
#565 = CARTESIAN_POINT ( 'NONE',  ( -3.749994990996019517, 3.750000832047212906, 17.65096039353565160 ) ) ;
#566 = VERTEX_POINT ( 'NONE', #1263 ) ;
#567 = VERTEX_POINT ( 'NONE', #2679 ) ;
#568 = AXIS2_PLACEMENT_3D ( 'NONE', #4180, #273, #2358 ) ;
#569 = UNCERTAINTY_MEASURE_WITH_UNIT (LENGTH_MEASURE( 1.000000000000000082E-05 ), #2969, 'distance_accuracy_value', 'NONE');
#570 = EDGE_LOOP ( 'NONE', ( #1120, #2843, #4288, #3872 ) ) ;
#571 = LINE ( 'NONE', #3818, #3067 ) ;
#572 = AXIS2_PLACEMENT_3D ( 'NONE', #953, #4576, #2038 ) ;
#573 = ADVANCED_FACE ( 'NONE', ( #4118 ), #2319, .F. ) ;
#574 =( LENGTH_UNIT ( ) NAMED_UNIT ( * ) SI_UNIT ( .MILLI., .METRE. ) );
#575 = CARTESIAN_POINT ( 'NONE',  ( -13.83934635305755378, -3.550665210907423930, 32.83413998674555501 ) ) ;
#576 = CARTESIAN_POINT ( 'NONE',  ( -14.28749276543804569, 0.004097986548671483757, 35.44137445358909133 ) ) ;
#577 = DIRECTION ( 'NONE',  ( -1.000000000000000000, -0.000000000000000000, -0.000000000000000000 ) ) ;
#578 = CIRCLE ( 'NONE', #4186, 0.7499999999999997780 ) ;
#579 = VECTOR ( 'NONE', #1317, 1000.000000000000000 ) ;
#580 = CARTESIAN_POINT ( 'NONE',  ( -13.83947632439384812, -3.546053490249568618, 31.39589353661586557 ) ) ;
#581 = ORIENTED_EDGE ( 'NONE', *, *, #1923, .F. ) ;
#582 = CARTESIAN_POINT ( 'NONE',  ( 17.28000050552179445, -3.039999999999999591, 17.28000050552179445 ) ) ;
#583 = CARTESIAN_POINT ( 'NONE',  ( -11.90638613189174144, -7.897499167952782173, 17.65096039353565160 ) ) ;
#584 = ORIENTED_EDGE ( 'NONE', *, *, #4023, .T. ) ;
#585 = DIRECTION ( 'NONE',  ( -8.673617379884035472E-16, -1.000000000000000000, -0.000000000000000000 ) ) ;
#586 = VECTOR ( 'NONE', #1807, 1000.000000000000000 ) ;
#587 = DIRECTION ( 'NONE',  ( 0.000000000000000000, -0.000000000000000000, -1.000000000000000000 ) ) ;
#588 = ORIENTED_EDGE ( 'NONE', *, *, #2678, .T. ) ;
#589 = ORIENTED_EDGE ( 'NONE', *, *, #3566, .T. ) ;
#590 = FILL_AREA_STYLE_COLOUR ( '', #4459 ) ;
#591 = EDGE_CURVE ( 'NONE', #2688, #3887, #2455, .T. ) ;
#592 = VECTOR ( 'NONE', #3864, 1000.000000000000000 ) ;
#593 = ORIENTED_EDGE ( 'NONE', *, *, #2041, .F. ) ;
#594 = DIRECTION ( 'NONE',  ( -1.000000000000000000, 1.076498916035107744E-16, 0.000000000000000000 ) ) ;
#595 = DIRECTION ( 'NONE',  ( 1.000000000000000000, 8.673617379884035472E-17, -0.000000000000000000 ) ) ;
#596 = PRODUCT_DEFINITION_SHAPE ( 'NONE', 'NONE',  #4661 ) ;
#597 = CARTESIAN_POINT ( 'NONE',  ( -12.58214063916086722, -6.772262032262147180, 34.69848916189056354 ) ) ;
#598 = CARTESIAN_POINT ( 'NONE',  ( 13.60368842669744538, -4.371226900785080360, 38.02566532807936994 ) ) ;
#599 = DIRECTION ( 'NONE',  ( 9.517981353260378315E-33, 8.841607930564763213E-17, -1.000000000000000000 ) ) ;
#600 = EDGE_CURVE ( 'NONE', #2299, #1212, #1035, .T. ) ;
#601 = EDGE_CURVE ( 'NONE', #1592, #1729, #2328, .T. ) ;
#602 = CARTESIAN_POINT ( 'NONE',  ( -14.20090908106113403, -1.585388553952144175, 29.15464480295243277 ) ) ;
#603 = CARTESIAN_POINT ( 'NONE',  ( 17.78000050552179445, -10.16000000000000014, 13.73375050552179744 ) ) ;
#604 = ORIENTED_EDGE ( 'NONE', *, *, #1834, .F. ) ;
#605 = CARTESIAN_POINT ( 'NONE',  ( 2.316727177394500794E-17, 0.000000000000000000, 1.587499999999999467 ) ) ;
#606 = EDGE_CURVE ( 'NONE', #1954, #21, #4612, .T. ) ;
#607 = CIRCLE ( 'NONE', #3547, 0.5000000000000004441 ) ;
#608 = ORIENTED_EDGE ( 'NONE', *, *, #1858, .F. ) ;
#609 = AXIS2_PLACEMENT_3D ( 'NONE', #1952, #2354, #4060 ) ;
#610 = DIRECTION ( 'NONE',  ( 1.000000000000000000, 0.000000000000000000, -0.000000000000000000 ) ) ;
#611 = PRODUCT ( 'Part 135_Varsay\X2\0131\X0\lan', 'Part 135_Varsay\X2\0131\X0\lan', '', ( #3231 ) ) ;
#612 = CARTESIAN_POINT ( 'NONE',  ( 3.040000505521796015, -2.539999999999999591, 17.28000050552179445 ) ) ;
#613 = CIRCLE ( 'NONE', #1794, 6.397499999999999964 ) ;
#614 = ORIENTED_EDGE ( 'NONE', *, *, #2744, .F. ) ;
#615 = ORIENTED_EDGE ( 'NONE', *, *, #4312, .F. ) ;
#616 = CIRCLE ( 'NONE', #1458, 14.28750000000000142 ) ;
#617 = CARTESIAN_POINT ( 'NONE',  ( 3.750005009003979595, -3.749999167952787538, 18.79096039353565217 ) ) ;
#618 = ORIENTED_EDGE ( 'NONE', *, *, #1715, .F. ) ;
#619 = DIRECTION ( 'NONE',  ( -0.000000000000000000, 1.000000000000000000, -0.000000000000000000 ) ) ;
#620 = CARTESIAN_POINT ( 'NONE',  ( -8.423108025121083031, 18.01695892724079684, 56.18096039353566340 ) ) ;
#621 =( GEOMETRIC_REPRESENTATION_CONTEXT ( 3 ) GLOBAL_UNCERTAINTY_ASSIGNED_CONTEXT ( ( #4151 ) ) GLOBAL_UNIT_ASSIGNED_CONTEXT ( ( #3277, #2536, #4002 ) ) REPRESENTATION_CONTEXT ( 'NONE', 'WORKASPACE' ) );
#622 = CARTESIAN_POINT ( 'NONE',  ( -12.37116712624658810, -7.147499167952783061, 32.36596039353565857 ) ) ;
#623 = CARTESIAN_POINT ( 'NONE',  ( 12.47854901097075597, -6.958554981044172472, 34.01560235227155715 ) ) ;
#624 =( NAMED_UNIT ( * ) PLANE_ANGLE_UNIT ( ) SI_UNIT ( $, .RADIAN. ) );
#625 = CARTESIAN_POINT ( 'NONE',  ( 14.28750500900398279, 8.320472145953950175E-07, 35.93971039353566965 ) ) ;
#626 = FACE_OUTER_BOUND ( 'NONE', #1636, .T. ) ;
#627 = ORIENTED_EDGE ( 'NONE', *, *, #591, .F. ) ;
#628 = CARTESIAN_POINT ( 'NONE',  ( -7.619994990996021400, -7.147499167952783061, 18.40096039353565160 ) ) ;
#629 = DIRECTION ( 'NONE',  ( -1.000000000000000000, 0.000000000000000000, 0.000000000000000000 ) ) ;
#630 = ORIENTED_EDGE ( 'NONE', *, *, #59, .F. ) ;
#631 = CARTESIAN_POINT ( 'NONE',  ( -17.48249499099600968, -7.147499167952783061, 32.36596039353565857 ) ) ;
#632 = CARTESIAN_POINT ( 'NONE',  ( 7.234561953626996335E-06, 0.004097986548672528061, -8.542375546410942988 ) ) ;
#633 = ORIENTED_EDGE ( 'NONE', *, *, #3448, .F. ) ;
#634 = ORIENTED_EDGE ( 'NONE', *, *, #547, .F. ) ;
#635 = EDGE_LOOP ( 'NONE', ( #3645, #633, #1686, #3639, #3220 ) ) ;
#636 = DIRECTION ( 'NONE',  ( -0.000000000000000000, -0.000000000000000000, 1.000000000000000000 ) ) ;
#637 = CARTESIAN_POINT ( 'NONE',  ( 13.83333536583607781, -3.569652013451328543, 31.86762445358909446 ) ) ;
#638 = CLOSED_SHELL ( 'NONE', ( #3107, #3851, #4206, #671 ) ) ;
#639 = DIRECTION ( 'NONE',  ( 0.000000000000000000, 0.000000000000000000, 1.000000000000000000 ) ) ;
#640 = CARTESIAN_POINT ( 'NONE',  ( -13.48443333977609626, -4.726286587311965270, 37.73272338279510763 ) ) ;
#641 = FACE_OUTER_BOUND ( 'NONE', #1386, .T. ) ;
#642 = CARTESIAN_POINT ( 'NONE',  ( -7.619994990996021400, -6.397499167952784838, 17.65096039353565160 ) ) ;
#643 = EDGE_CURVE ( 'NONE', #2188, #2506, #1347, .T. ) ;
#644 = ADVANCED_FACE ( 'NONE', ( #1639 ), #1439, .T. ) ;
#645 = VECTOR ( 'NONE', #1619, 1000.000000000000000 ) ;
#646 = CARTESIAN_POINT ( 'NONE',  ( -3.749999999999999556, -3.750000000000000888, 146.2500000000000000 ) ) ;
#647 = EDGE_CURVE ( 'NONE', #2212, #1270, #1398, .T. ) ;
#648 = DIRECTION ( 'NONE',  ( 1.000000000000000000, 0.000000000000000000, 0.000000000000000000 ) ) ;
#649 = CARTESIAN_POINT ( 'NONE',  ( 3.040000505521796015, -17.28000000000000114, 17.78000050552179445 ) ) ;
#650 = DIRECTION ( 'NONE',  ( 0.000000000000000000, 0.000000000000000000, 1.000000000000000000 ) ) ;
#651 = AXIS2_PLACEMENT_3D ( 'NONE', #3780, #4442, #484 ) ;
#652 = CARTESIAN_POINT ( 'NONE',  ( -8.369994990996019624, 8.320472137110901854E-07, 32.36596039353565857 ) ) ;
#653 = ORIENTED_EDGE ( 'NONE', *, *, #499, .F. ) ;
#654 = CARTESIAN_POINT ( 'NONE',  ( -11.90638390633376709, -7.893402013451320975, 17.15262445358908039 ) ) ;
#655 = FACE_OUTER_BOUND ( 'NONE', #122, .T. ) ;
#656 = FACE_OUTER_BOUND ( 'NONE', #2707, .T. ) ;
#657 = VERTEX_POINT ( 'NONE', #327 ) ;
#658 = ORIENTED_EDGE ( 'NONE', *, *, #1152, .F. ) ;
#659 = EDGE_CURVE ( 'NONE', #2566, #1592, #1893, .T. ) ;
#660 = DIRECTION ( 'NONE',  ( 1.000000000000000000, 0.000000000000000000, 0.000000000000000000 ) ) ;
#661 = AXIS2_PLACEMENT_3D ( 'NONE', #2914, #1638, #3650 ) ;
#662 = ORIENTED_EDGE ( 'NONE', *, *, #4578, .T. ) ;
#663 = CARTESIAN_POINT ( 'NONE',  ( -8.369992765438043492, 6.401597986548673624, 17.15262445358908039 ) ) ;
#664 = ORIENTED_EDGE ( 'NONE', *, *, #3366, .T. ) ;
#665 = LINE ( 'NONE', #4242, #2306 ) ;
#666 = DIRECTION ( 'NONE',  ( -1.000000000000000000, 1.076498916035098007E-16, 1.723826117363954227E-31 ) ) ;
#667 = EDGE_CURVE ( 'NONE', #3496, #2728, #3377, .T. ) ;
#668 = CARTESIAN_POINT ( 'NONE',  ( -12.39925909105915736, -7.099459522532631794, 33.31797499930306827 ) ) ;
#669 = TOROIDAL_SURFACE ( 'NONE', #3076, 1.500000000000000000, 0.7500000000000000000 ) ;
#670 = DIRECTION ( 'NONE',  ( 1.000000000000000000, 0.000000000000000000, 0.000000000000000000 ) ) ;
#671 = ADVANCED_FACE ( 'NONE', ( #3174 ), #2134, .F. ) ;
#672 = CARTESIAN_POINT ( 'NONE',  ( -14.28749499099602360, 0.2337324564415137751, 28.79221039353567591 ) ) ;
#673 = DIRECTION ( 'NONE',  ( 0.000000000000000000, 0.000000000000000000, 1.000000000000000000 ) ) ;
#674 = CARTESIAN_POINT ( 'NONE',  ( -8.369992765438045268, -7.143402013451323640, 17.90262445358908039 ) ) ;
#675 = VERTEX_POINT ( 'NONE', #984 ) ;
#676 = CARTESIAN_POINT ( 'NONE',  ( 12.39929365807998884, -7.095336152118751016, 32.82105853334657297 ) ) ;
#677 = AXIS2_PLACEMENT_3D ( 'NONE', #2160, #3273, #1114 ) ;
#678 = DIRECTION ( 'NONE',  ( 0.000000000000000000, 0.000000000000000000, -1.000000000000000000 ) ) ;
#679 = VECTOR ( 'NONE', #2972, 1000.000000000000000 ) ;
#680 = VERTEX_POINT ( 'NONE', #2071 ) ;
#681 = AXIS2_PLACEMENT_3D ( 'NONE', #97, #142, #475 ) ;
#682 = ORIENTED_EDGE ( 'NONE', *, *, #406, .T. ) ;
#683 = AXIS2_PLACEMENT_3D ( 'NONE', #882, #3332, #1973 ) ;
#684 = ORIENTED_EDGE ( 'NONE', *, *, #1424, .T. ) ;
#685 = ORIENTED_EDGE ( 'NONE', *, *, #526, .T. ) ;
#686 = CARTESIAN_POINT ( 'NONE',  ( -14.28749276543804925, 0.004097986548672528061, 28.29387445358909403 ) ) ;
#687 = PRODUCT_CONTEXT ( 'NONE', #2013, 'mechanical' ) ;
#688 = CARTESIAN_POINT ( 'NONE',  ( -3.152215195724335839, -3.565902013451327068, -8.542375546410942988 ) ) ;
#689 = CARTESIAN_POINT ( 'NONE',  ( 13.87988099929733110, -3.389724456514533912, 31.20998424916602332 ) ) ;
#690 = DIRECTION ( 'NONE',  ( -0.000000000000000000, -1.000000000000000000, -0.000000000000000000 ) ) ;
#691 = CARTESIAN_POINT ( 'NONE',  ( -13.83947854995182247, -3.550150644751030260, 31.89422947656246521 ) ) ;
#692 = DIRECTION ( 'NONE',  ( -0.000000000000000000, -0.000000000000000000, -1.000000000000000000 ) ) ;
#693 = DIRECTION ( 'NONE',  ( -0.000000000000000000, 0.000000000000000000, -1.000000000000000000 ) ) ;
#694 = DIRECTION ( 'NONE',  ( 1.000000000000000000, -1.076498916035107621E-16, 0.000000000000000000 ) ) ;
#695 = DIRECTION ( 'NONE',  ( -1.000000000000000000, 1.076498916035107621E-16, -0.000000000000000000 ) ) ;
#696 = VERTEX_POINT ( 'NONE', #3528 ) ;
#697 = CARTESIAN_POINT ( 'NONE',  ( 14.28750723456195537, 0.004097986548674278397, 39.01512445358908820 ) ) ;
#698 = VECTOR ( 'NONE', #4638, 1000.000000000000000 ) ;
#699 = PRODUCT_RELATED_PRODUCT_CATEGORY ( 'part', '', ( #2825 ) ) ;
#700 = FACE_OUTER_BOUND ( 'NONE', #2771, .T. ) ;
#701 = ORIENTED_EDGE ( 'NONE', *, *, #3222, .T. ) ;
#702 = EDGE_LOOP ( 'NONE', ( #2986, #2462, #3719, #3899 ) ) ;
#703 = B_SPLINE_CURVE_WITH_KNOTS ( 'NONE', 3,
 ( #932, #459, #2970, #2270, #1000, #1696, #291, #1716, #4604, #4244 ),
 .UNSPECIFIED., .F., .F.,
 ( 4, 2, 2, 2, 4 ),
 ( 0.000000000000000000, 0.0003199342119934979684, 0.0006398684239869959368, 0.0009598026359804939052, 0.001279736847973991874 ),
 .UNSPECIFIED. ) ;
#704 = CARTESIAN_POINT ( 'NONE',  ( 12.37117714425454551, 7.147500832047207098, 17.65096039353565160 ) ) ;
#705 = ORIENTED_EDGE ( 'NONE', *, *, #163, .F. ) ;
#706 = DIRECTION ( 'NONE',  ( -1.000000000000000000, 0.000000000000000000, 0.000000000000000000 ) ) ;
#707 = EDGE_LOOP ( 'NONE', ( #524, #3331, #1259 ) ) ;
#708 = DIRECTION ( 'NONE',  ( 1.076498916035107744E-16, 1.000000000000000000, 0.000000000000000000 ) ) ;
#709 = CARTESIAN_POINT ( 'NONE',  ( 12.58215288272680255, 6.776360850858033302, 34.20015322194399232 ) ) ;
#710 = CARTESIAN_POINT ( 'NONE',  ( 14.24236565909520280, -1.155183429066308998, 28.97606331622595732 ) ) ;
#711 = AXIS2_PLACEMENT_3D ( 'NONE', #2375, #639, #4553 ) ;
#712 = EDGE_CURVE ( 'NONE', #566, #2813, #3871, .T. ) ;
#713 = CARTESIAN_POINT ( 'NONE',  ( -14.25898160115544933, 0.9311474368774493859, 28.90767711873708734 ) ) ;
#714 = CARTESIAN_POINT ( 'NONE',  ( -12.37116490068861197, -7.143402013451323640, 31.86762445358908735 ) ) ;
#715 = DIRECTION ( 'NONE',  ( 0.000000000000000000, 0.000000000000000000, -1.000000000000000000 ) ) ;
#716 = DIRECTION ( 'NONE',  ( 1.707404996040164265E-16, -1.000000000000000000, -0.000000000000000000 ) ) ;
#717 = VECTOR ( 'NONE', #433, 1000.000000000000000 ) ;
#718 = CARTESIAN_POINT ( 'NONE',  ( -14.28749276543804925, 0.004097986548672528061, 28.29387445358909403 ) ) ;
#719 = VERTEX_POINT ( 'NONE', #2408 ) ;
#720 = CARTESIAN_POINT ( 'NONE',  ( 14.28155188315728807, 0.4717409201294489041, 35.91611237606498719 ) ) ;
#721 = CYLINDRICAL_SURFACE ( 'NONE', #3310, 0.7499999999999997780 ) ;
#722 = AXIS2_PLACEMENT_3D ( 'NONE', #3419, #193, #1172 ) ;
#723 = ORIENTED_EDGE ( 'NONE', *, *, #4476, .T. ) ;
#724 = VERTEX_POINT ( 'NONE', #3197 ) ;
#725 = CARTESIAN_POINT ( 'NONE',  ( -14.17127587220999274, 1.881159699106039751, 38.78036386370911970 ) ) ;
#726 = VECTOR ( 'NONE', #2088, 1000.000000000000000 ) ;
#727 = ORIENTED_EDGE ( 'NONE', *, *, #1424, .F. ) ;
#728 = VERTEX_POINT ( 'NONE', #674 ) ;
#729 = DIRECTION ( 'NONE',  ( -1.000000000000000000, 0.000000000000000000, 0.000000000000000000 ) ) ;
#730 = DIRECTION ( 'NONE',  ( -1.040834085586084257E-17, 0.000000000000000000, 1.000000000000000000 ) ) ;
#731 = CARTESIAN_POINT ( 'NONE',  ( 14.28750500900398279, 8.320472145597748469E-07, 28.79221039353566880 ) ) ;
#732 = CIRCLE ( 'NONE', #2241, 0.5000000000000000000 ) ;
#733 = CARTESIAN_POINT ( 'NONE',  ( -0.5650967372767217167, -3.565902013451328401, -9.700646504717855834 ) ) ;
#734 = EDGE_CURVE ( 'NONE', #1942, #3678, #1058, .T. ) ;
#735 = CARTESIAN_POINT ( 'NONE',  ( 8.370007234561949616, -7.143402013451325416, 17.90262445358908039 ) ) ;
#736 = CARTESIAN_POINT ( 'NONE',  ( -13.83332312227014427, 3.573750832047214221, 32.13187428197717566 ) ) ;
#737 = FACE_BOUND ( 'NONE', #3749, .T. ) ;
#738 = FACE_BOUND ( 'NONE', #4116, .T. ) ;
#739 = CARTESIAN_POINT ( 'NONE',  ( 13.83333536583607959, -3.569652013451329431, 32.10466053564423561 ) ) ;
#740 =( LENGTH_UNIT ( ) NAMED_UNIT ( * ) SI_UNIT ( .MILLI., .METRE. ) );
#741 = EDGE_CURVE ( 'NONE', #3225, #2052, #2478, .T. ) ;
#742 = PLANE ( 'NONE',  #2974 ) ;
#743 = EDGE_CURVE ( 'NONE', #3745, #4049, #1749, .T. ) ;
#744 = VERTEX_POINT ( 'NONE', #1184 ) ;
#745 = CARTESIAN_POINT ( 'NONE',  ( -13.83332089671217169, 3.577847986548673642, 31.86762445358909446 ) ) ;
#746 = DIRECTION ( 'NONE',  ( 0.000000000000000000, -1.000000000000000000, 0.000000000000000000 ) ) ;
#747 = EDGE_CURVE ( 'NONE', #1143, #3946, #4587, .T. ) ;
#748 = EDGE_CURVE ( 'NONE', #2770, #4203, #1083, .T. ) ;
#749 = CIRCLE ( 'NONE', #3983, 0.5000000000000004441 ) ;
#750 = DIRECTION ( 'NONE',  ( 1.076498916035107744E-16, 1.000000000000000000, 0.000000000000000000 ) ) ;
#751 = ORIENTED_EDGE ( 'NONE', *, *, #2927, .F. ) ;
#752 = ORIENTED_EDGE ( 'NONE', *, *, #1769, .F. ) ;
#753 = VECTOR ( 'NONE', #4301, 1000.000000000000000 ) ;
#754 = EDGE_LOOP ( 'NONE', ( #2143, #4391, #2842, #2593 ) ) ;
#755 = ORIENTED_EDGE ( 'NONE', *, *, #3251, .T. ) ;
#756 = AXIS2_PLACEMENT_3D ( 'NONE', #1719, #3434, #648 ) ;
#757 = CYLINDRICAL_SURFACE ( 'NONE', #1661, 14.28750000000000142 ) ;
#758 = PRODUCT_CONTEXT ( 'NONE', #324, 'mechanical' ) ;
#759 = CARTESIAN_POINT ( 'NONE',  ( 14.16479288468515207, 1.886616767965749286, 38.76682706999739736 ) ) ;
#760 = CARTESIAN_POINT ( 'NONE',  ( 14.99250500900398109, 7.147500832047209762, 3.790960393535649064 ) ) ;
#761 = CARTESIAN_POINT ( 'NONE',  ( -8.369994990996016071, 7.897500832047212427, 18.40096039353565160 ) ) ;
#762 = CYLINDRICAL_SURFACE ( 'NONE', #4557, 0.5000000000000004441 ) ;
#763 = DIRECTION ( 'NONE',  ( 0.000000000000000000, 0.000000000000000000, 1.000000000000000000 ) ) ;
#764 = CARTESIAN_POINT ( 'NONE',  ( -14.00282210529756277, -2.836878008355436798, 34.04832179759813471 ) ) ;
#765 = DIRECTION ( 'NONE',  ( 0.000000000000000000, 0.000000000000000000, -1.000000000000000000 ) ) ;
#766 = ORIENTED_EDGE ( 'NONE', *, *, #3357, .F. ) ;
#767 = LINE ( 'NONE', #1864, #3140 ) ;
#768 = CARTESIAN_POINT ( 'NONE',  ( -14.28749276543804925, 0.004097986548672528061, 39.01512445358908820 ) ) ;
#769 = ADVANCED_FACE ( 'NONE', ( #1985 ), #4591, .T. ) ;
#770 = VECTOR ( 'NONE', #3536, 1000.000000000000000 ) ;
#771 = CARTESIAN_POINT ( 'NONE',  ( 3.749999999999999556, -3.750000000000000888, 3.749999999999995559 ) ) ;
#772 = ORIENTED_EDGE ( 'NONE', *, *, #1281, .F. ) ;
#773 = EDGE_CURVE ( 'NONE', #849, #4505, #1374, .T. ) ;
#774 = ORIENTED_EDGE ( 'NONE', *, *, #2076, .F. ) ;
#775 = CARTESIAN_POINT ( 'NONE',  ( -14.28749276543804925, 0.004097986548672528061, 39.01512445358908820 ) ) ;
#776 = ORIENTED_EDGE ( 'NONE', *, *, #429, .F. ) ;
#777 = CARTESIAN_POINT ( 'NONE',  ( 2.316727177394501718E-17, 0.000000000000000000, 33.33750000000000568 ) ) ;
#778 = PRODUCT_CONTEXT ( 'NONE', #1536, 'mechanical' ) ;
#779 = CARTESIAN_POINT ( 'NONE',  ( 14.25899708262535803, 0.9309096077285254900, 28.90765582148817714 ) ) ;
#780 = CARTESIAN_POINT ( 'NONE',  ( 14.09723484945316763, 2.339307409763772938, 38.62703793808391595 ) ) ;
#781 = LINE ( 'NONE', #4057, #1971 ) ;
#782 = CARTESIAN_POINT ( 'NONE',  ( -8.369992765438038163, 7.151597986548673624, 31.86762445358908735 ) ) ;
#783 = DIRECTION ( 'NONE',  ( 1.000000000000000000, 0.000000000000000000, -0.000000000000000000 ) ) ;
#784 = ADVANCED_FACE ( 'NONE', ( #785 ), #64, .T. ) ;
#785 = FACE_OUTER_BOUND ( 'NONE', #2617, .T. ) ;
#786 = FACE_OUTER_BOUND ( 'NONE', #4051, .T. ) ;
#787 = PRODUCT_DEFINITION_FORMATION_WITH_SPECIFIED_SOURCE ( 'ANY', '', #4598, .NOT_KNOWN. ) ;
#788 = ORIENTED_EDGE ( 'NONE', *, *, #1129, .F. ) ;
#789 = CARTESIAN_POINT ( 'NONE',  ( 14.09171514697193039, 2.363129204819476303, 35.05698690432073761 ) ) ;
#790 = CIRCLE ( 'NONE', #198, 0.5000000000000000000 ) ;
#791 = CARTESIAN_POINT ( 'NONE',  ( -12.87894808284510795, -6.188309651760397934, 35.46704985752301553 ) ) ;
#792 = EDGE_CURVE ( 'NONE', #4332, #744, #3761, .T. ) ;
#793 = LINE ( 'NONE', #1935, #2576 ) ;
#794 = EDGE_LOOP ( 'NONE', ( #3294, #1826, #3928, #916 ) ) ;
#795 = FACE_OUTER_BOUND ( 'NONE', #3698, .T. ) ;
#796 = CIRCLE ( 'NONE', #4183, 0.7500000000000006661 ) ;
#797 = FACE_OUTER_BOUND ( 'NONE', #2697, .T. ) ;
#798 = CARTESIAN_POINT ( 'NONE',  ( 3.573749999999998650, 4.376581498452851814E-16, 11.11249999999999893 ) ) ;
#799 = TOROIDAL_SURFACE ( 'NONE', #4032, 6.397499999999999964, 0.7500000000000000000 ) ;
#800 = DIRECTION ( 'NONE',  ( -1.000000000000000000, 0.000000000000000000, 0.000000000000000000 ) ) ;
#801 = ORIENTED_EDGE ( 'NONE', *, *, #3259, .T. ) ;
#802 = ORIENTED_EDGE ( 'NONE', *, *, #395, .T. ) ;
#803 = CARTESIAN_POINT ( 'NONE',  ( -14.09151346090570378, 2.364225744170925569, 35.05594847197529873 ) ) ;
#804 = ITEM_DEFINED_TRANSFORMATION ( 'NONE', 'NONE', #4248,  #4483 ) ;
#805 = LINE ( 'NONE', #3748, #9 ) ;
#806 = VECTOR ( 'NONE', #1352, 1000.000000000000000 ) ;
#807 = ORIENTED_EDGE ( 'NONE', *, *, #3353, .T. ) ;
#808 = ADVANCED_FACE ( 'NONE', ( #2224 ), #16, .F. ) ;
#809 = SURFACE_STYLE_FILL_AREA ( #1922 ) ;
#810 = EDGE_CURVE ( 'NONE', #1644, #3603, #2778, .T. ) ;
#811 = LINE ( 'NONE', #3777, #899 ) ;
#812 = FACE_OUTER_BOUND ( 'NONE', #3133, .T. ) ;
#813 = AXIS2_PLACEMENT_3D ( 'NONE', #362, #729, #1021 ) ;
#814 = DIRECTION ( 'NONE',  ( -0.000000000000000000, -0.000000000000000000, -1.000000000000000000 ) ) ;
#815 = EDGE_LOOP ( 'NONE', ( #4486, #2215 ) ) ;
#816 = CARTESIAN_POINT ( 'NONE',  ( 2.316727177394501718E-17, 0.000000000000000000, 33.33750000000000568 ) ) ;
#817 = DIRECTION ( 'NONE',  ( 1.000000000000000000, 0.000000000000000000, -0.000000000000000000 ) ) ;
#818 = AXIS2_PLACEMENT_3D ( 'NONE', #3591, #1859, #4322 ) ;
#819 = ORIENTED_EDGE ( 'NONE', *, *, #3769, .T. ) ;
#820 = DIRECTION ( 'NONE',  ( 1.000000000000000000, -1.076498916035107621E-16, 0.000000000000000000 ) ) ;
#821 = DIRECTION ( 'NONE',  ( 0.7071067811865449082, 0.000000000000000000, 0.7071067811865501263 ) ) ;
#822 = CARTESIAN_POINT ( 'NONE',  ( 13.85858879626102791, 3.483479532322464323, 32.80720252877481613 ) ) ;
#823 = ORIENTED_EDGE ( 'NONE', *, *, #3835, .T. ) ;
#824 = ORIENTED_EDGE ( 'NONE', *, *, #1700, .T. ) ;
#825 = DIRECTION ( 'NONE',  ( 1.076498916035107621E-16, 1.000000000000000000, -0.000000000000000000 ) ) ;
#826 = AXIS2_PLACEMENT_3D ( 'NONE', #3565, #3822, #2806 ) ;
#827 = DIRECTION ( 'NONE',  ( -1.000000000000000000, 1.076498916035107621E-16, -0.000000000000000000 ) ) ;
#828 = EDGE_CURVE ( 'NONE', #744, #2975, #2549, .T. ) ;
#829 = AXIS2_PLACEMENT_3D ( 'NONE', #3408, #3755, #2694 ) ;
#830 = CARTESIAN_POINT ( 'NONE',  ( 17.28000050552179800, -17.28000000000000114, 3.040000505521796015 ) ) ;
#831 = PLANE ( 'NONE',  #985 ) ;
#832 = SHAPE_REPRESENTATION_RELATIONSHIP ( 'NONE' , 'NONE' ,  #2003, #2068 ) ;
#833 = CARTESIAN_POINT ( 'NONE',  ( 7.234561953626996335E-06, 0.004097986548672528061, -10.04237554641092345 ) ) ;
#834 = DIRECTION ( 'NONE',  ( 0.000000000000000000, 0.000000000000000000, -1.000000000000000000 ) ) ;
#835 = CARTESIAN_POINT ( 'NONE',  ( -3.749994990996019961, -3.749999167952787094, 18.79096039353565217 ) ) ;
#836 = CIRCLE ( 'NONE', #1069, 0.7500000000000006661 ) ;
#837 = EDGE_LOOP ( 'NONE', ( #1147, #281, #4283, #4594 ) ) ;
#838 = DIRECTION ( 'NONE',  ( 0.000000000000000000, 0.000000000000000000, -1.000000000000000000 ) ) ;
#839 = VECTOR ( 'NONE', #2316, 1000.000000000000000 ) ;
#840 = CARTESIAN_POINT ( 'NONE',  ( 14.09176851988465629, 2.366970977748110716, 29.17628584082743259 ) ) ;
#841 = CARTESIAN_POINT ( 'NONE',  ( -8.369994990996019624, -6.397499167952784838, 18.40096039353565160 ) ) ;
#842 = ORIENTED_EDGE ( 'NONE', *, *, #3937, .T. ) ;
#843 = FACE_OUTER_BOUND ( 'NONE', #264, .T. ) ;
#844 = DIRECTION ( 'NONE',  ( -1.000000000000000000, 0.000000000000000000, 0.000000000000000000 ) ) ;
#845 = DIRECTION ( 'NONE',  ( -1.000000000000000000, 0.000000000000000000, 0.000000000000000000 ) ) ;
#846 = EDGE_CURVE ( 'NONE', #4649, #313, #2557, .T. ) ;
#847 = CARTESIAN_POINT ( 'NONE',  ( 14.28750723456195537, 0.004097986548674313959, 35.44137445358909133 ) ) ;
#848 = ADVANCED_FACE ( 'NONE', ( #812 ), #3681, .T. ) ;
#849 = VERTEX_POINT ( 'NONE', #718 ) ;
#850 = ORIENTED_EDGE ( 'NONE', *, *, #667, .T. ) ;
#851 = CONTEXT_DEPENDENT_SHAPE_REPRESENTATION ( #4563, #1680 ) ;
#852 = DIRECTION ( 'NONE',  ( -1.000000000000000000, 1.076498916035107744E-16, 0.000000000000000000 ) ) ;
#853 = AXIS2_PLACEMENT_3D ( 'NONE', #2532, #750, #2185 ) ;
#854 = ADVANCED_FACE ( 'NONE', ( #2156 ), #4440, .F. ) ;
#855 = CARTESIAN_POINT ( 'NONE',  ( 8.370005009003978813, -7.897499167952783949, 18.40096039353565160 ) ) ;
#856 = ORIENTED_EDGE ( 'NONE', *, *, #3651, .F. ) ;
#857 = CARTESIAN_POINT ( 'NONE',  ( -12.47853899296279501, 6.958556645138596508, 34.01560235227155715 ) ) ;
#858 =( NAMED_UNIT ( * ) PLANE_ANGLE_UNIT ( ) SI_UNIT ( $, .RADIAN. ) );
#859 =( NAMED_UNIT ( * ) PLANE_ANGLE_UNIT ( ) SI_UNIT ( $, .RADIAN. ) );
#860 = CARTESIAN_POINT ( 'NONE',  ( -7.619992765438045268, 0.004097986548673348585, 31.86762445358909446 ) ) ;
#861 = DIRECTION ( 'NONE',  ( 1.000000000000000000, 0.000000000000000000, 0.000000000000000000 ) ) ;
#862 = CARTESIAN_POINT ( 'NONE',  ( 18.74250500900397753, 3.573750832047210224, 32.36596039353566567 ) ) ;
#863 = ORIENTED_EDGE ( 'NONE', *, *, #344, .F. ) ;
#864 = CARTESIAN_POINT ( 'NONE',  ( 12.37117936981252164, -7.143402013451325416, 17.90262445358908039 ) ) ;
#865 = EDGE_CURVE ( 'NONE', #3460, #1305, #1452, .T. ) ;
#866 = DIRECTION ( 'NONE',  ( 1.000000000000000000, 1.076498916035107621E-16, -0.000000000000000000 ) ) ;
#867 = DIRECTION ( 'NONE',  ( 0.000000000000000000, 0.000000000000000000, 1.000000000000000000 ) ) ;
#868 = EDGE_LOOP ( 'NONE', ( #3791, #1806, #856, #2282 ) ) ;
#869 = CARTESIAN_POINT ( 'NONE',  ( 13.73375050552179566, -8.066545718530848674, 13.73375050552179566 ) ) ;
#870 = EDGE_CURVE ( 'NONE', #1869, #2259, #225, .T. ) ;
#871 = EDGE_CURVE ( 'NONE', #313, #4140, #2012, .T. ) ;
#872 = CARTESIAN_POINT ( 'NONE',  ( -6.869994990996020512, 8.320472135496153183E-07, 17.65096039353565160 ) ) ;
#873 = CARTESIAN_POINT ( 'NONE',  ( 14.25909360596529041, 0.9333857149738187253, 35.32631526480061979 ) ) ;
#874 = AXIS2_PLACEMENT_3D ( 'NONE', #2902, #1555, #1883 ) ;
#875 = ORIENTED_EDGE ( 'NONE', *, *, #1369, .T. ) ;
#876 = ORIENTED_EDGE ( 'NONE', *, *, #542, .F. ) ;
#877 = CONTEXT_DEPENDENT_SHAPE_REPRESENTATION ( #3600, #2745 ) ;
#878 = DIRECTION ( 'NONE',  ( 0.000000000000000000, 1.000000000000000000, 0.000000000000000000 ) ) ;
#879 = DIRECTION ( 'NONE',  ( 1.000000000000000000, -1.076498916035107621E-16, -0.000000000000000000 ) ) ;
#880 = ORIENTED_EDGE ( 'NONE', *, *, #1621, .T. ) ;
#881 = CARTESIAN_POINT ( 'NONE',  ( 8.370007234561953169, 7.151597986548671848, 31.86762445358908735 ) ) ;
#882 = CARTESIAN_POINT ( 'NONE',  ( -9.549434556529077899E-17, -3.249382362871961689E-18, 146.2500000000000000 ) ) ;
#883 = EDGE_CURVE ( 'NONE', #3060, #1630, #1523, .T. ) ;
#884 = CARTESIAN_POINT ( 'NONE',  ( 17.28000050552179800, -17.78000000000000114, 17.28000050552179445 ) ) ;
#885 = CARTESIAN_POINT ( 'NONE',  ( 13.48444335778406078, 4.726288251406393748, 37.73272338279511473 ) ) ;
#886 = FACE_OUTER_BOUND ( 'NONE', #2438, .T. ) ;
#887 = DIRECTION ( 'NONE',  ( 0.000000000000000000, 1.000000000000000000, 0.000000000000000000 ) ) ;
#888 = CIRCLE ( 'NONE', #1348, 3.573749999999999538 ) ;
#889 = ORIENTED_EDGE ( 'NONE', *, *, #2151, .F. ) ;
#890 = CARTESIAN_POINT ( 'NONE',  ( 3.749999999999999556, 3.750000000000000000, 3.749999999999995559 ) ) ;
#891 = CARTESIAN_POINT ( 'NONE',  ( 8.370007234561951392, 0.004097986548671627739, 31.86762445358908735 ) ) ;
#892 = AXIS2_PLACEMENT_3D ( 'NONE', #3068, #4511, #4154 ) ;
#893 = ADVANCED_FACE ( 'NONE', ( #534 ), #4490, .F. ) ;
#894 = EDGE_CURVE ( 'NONE', #2688, #4520, #1274, .T. ) ;
#895 = DIRECTION ( 'NONE',  ( -1.000000000000000000, -1.076498916035107621E-16, 0.000000000000000000 ) ) ;
#896 = EDGE_LOOP ( 'NONE', ( #76, #2578, #3022, #2141 ) ) ;
#897 = PLANE ( 'NONE',  #661 ) ;
#898 = CARTESIAN_POINT ( 'NONE',  ( -7.619994990996019624, 8.320472136303528048E-07, 32.36596039353566567 ) ) ;
#899 = VECTOR ( 'NONE', #1250, 1000.000000000000000 ) ;
#900 = EDGE_CURVE ( 'NONE', #2669, #1336, #234, .T. ) ;
#901 = CARTESIAN_POINT ( 'NONE',  ( 14.99250723456195544, 7.901597986548669184, 17.90262445358908039 ) ) ;
#902 = CIRCLE ( 'NONE', #4130, 0.5000000000000000000 ) ;
#903 = EDGE_LOOP ( 'NONE', ( #4589, #99, #2024, #2664 ) ) ;
#904 = ORIENTED_EDGE ( 'NONE', *, *, #3945, .F. ) ;
#905 = CARTESIAN_POINT ( 'NONE',  ( 8.370005009003978813, -7.147499167952784838, 18.40096039353565160 ) ) ;
#906 = UNCERTAINTY_MEASURE_WITH_UNIT (LENGTH_MEASURE( 1.000000000000000082E-05 ), #574, 'distance_accuracy_value', 'NONE');
#907 = AXIS2_PLACEMENT_3D ( 'NONE', #255, #1703, #3238 ) ;
#908 = ORIENTED_EDGE ( 'NONE', *, *, #3940, .T. ) ;
#909 = DIRECTION ( 'NONE',  ( 0.000000000000000000, 8.673617379884035472E-16, 1.000000000000000000 ) ) ;
#910 = CARTESIAN_POINT ( 'NONE',  ( 14.28750723456195537, 0.004097986548674313959, 35.44137445358909133 ) ) ;
#911 = AXIS2_PLACEMENT_3D ( 'NONE', #1773, #1007, #4275 ) ;
#912 = CARTESIAN_POINT ( 'NONE',  ( -14.03250527701334427, 2.696503014659202613, 34.22909654994315076 ) ) ;
#913 = DIRECTION ( 'NONE',  ( -1.000000000000000000, 1.076498916035107744E-16, 0.000000000000000000 ) ) ;
#914 = STYLED_ITEM ( 'NONE', ( #1109 ), #1920 ) ;
#915 = VECTOR ( 'NONE', #3007, 1000.000000000000000 ) ;
#916 = ORIENTED_EDGE ( 'NONE', *, *, #3259, .F. ) ;
#917 = CYLINDRICAL_SURFACE ( 'NONE', #358, 3.573749999999999538 ) ;
#918 = VECTOR ( 'NONE', #1102, 1000.000000000000000 ) ;
#919 = VERTEX_POINT ( 'NONE', #4627 ) ;
#920 = LINE ( 'NONE', #561, #1310 ) ;
#921 = EDGE_LOOP ( 'NONE', ( #1969, #3596, #1759, #1916 ) ) ;
#922 = LINE ( 'NONE', #4522, #4502 ) ;
#923 = EDGE_CURVE ( 'NONE', #675, #4505, #2472, .T. ) ;
#924 = CARTESIAN_POINT ( 'NONE',  ( 7.620005009003980589, -6.397499167952786614, 18.40096039353565160 ) ) ;
#925 = ADVANCED_FACE ( 'NONE', ( #4198 ), #2105, .T. ) ;
#926 = EDGE_LOOP ( 'NONE', ( #2588, #4099, #614, #3794, #1777, #942, #2345, #3510, #25, #928, #802, #3539, #3224, #2933, #1757, #1 ) ) ;
#927 = ORIENTED_EDGE ( 'NONE', *, *, #2777, .T. ) ;
#928 = ORIENTED_EDGE ( 'NONE', *, *, #286, .F. ) ;
#929 = CARTESIAN_POINT ( 'NONE',  ( 2.540000505521796015, -17.28000000000000114, 17.28000050552179445 ) ) ;
#930 = AXIS2_PLACEMENT_3D ( 'NONE', #2841, #1142, #4307 ) ;
#931 = DIRECTION ( 'NONE',  ( 1.000000000000000000, -0.000000000000000000, 0.000000000000000000 ) ) ;
#932 = CARTESIAN_POINT ( 'NONE',  ( -12.37116490068861019, 7.151597986548670072, 17.90262445358908039 ) ) ;
#933 = CARTESIAN_POINT ( 'NONE',  ( -13.87981558764485790, 3.394021350125140835, 33.02272327460092782 ) ) ;
#934 = CARTESIAN_POINT ( 'NONE',  ( 2.540000505521796015, -17.28000000000000114, 17.78000050552179445 ) ) ;
#935 = PLANE ( 'NONE',  #3809 ) ;
#936 = DIRECTION ( 'NONE',  ( 0.000000000000000000, 0.000000000000000000, -1.000000000000000000 ) ) ;
#937 = EDGE_LOOP ( 'NONE', ( #2882, #2819, #1887, #4599 ) ) ;
#938 = B_SPLINE_CURVE_WITH_KNOTS ( 'NONE', 3,
 ( #622, #3889, #668, #2735, #597, #4625, #4175, #958, #4579, #1339, #2104, #2064, #640, #224, #2756, #4197, #2394, #318, #1675, #1739, #2019, #3843, #1411, #1365 ),
 .UNSPECIFIED., .F., .F.,
 ( 4, 2, 2, 2, 2, 2, 2, 2, 2, 2, 2, 4 ),
 ( -0.01136693575711653602, -0.009946068787476960993, -0.008525201817837385967, -0.007104334848197810942, -0.006393901363378032103, -0.005683467878558252397, -0.004973034393738473558, -0.004262600908918695586, -0.002841733939279125765, -0.002131300454459342589, -0.001420866969639559413, 8.673617379884035472E-18 ),
 .UNSPECIFIED. ) ;
#939 = CARTESIAN_POINT ( 'NONE',  ( 3.040000505521796015, -3.039999999999999591, 3.040000505521795571 ) ) ;
#940 = EDGE_LOOP ( 'NONE', ( #1917, #3425, #308, #2711, #4407 ) ) ;
#941 = CARTESIAN_POINT ( 'NONE',  ( 2.540000505521796015, -3.039999999999999591, 3.040000505521795571 ) ) ;
#942 = ORIENTED_EDGE ( 'NONE', *, *, #923, .T. ) ;
#943 = DIRECTION ( 'NONE',  ( 0.000000000000000000, 0.000000000000000000, -1.000000000000000000 ) ) ;
#944 = ADVANCED_FACE ( 'NONE', ( #2395 ), #1340, .T. ) ;
#945 = DIRECTION ( 'NONE',  ( 0.000000000000000000, -0.000000000000000000, -1.000000000000000000 ) ) ;
#946 = AXIS2_PLACEMENT_3D ( 'NONE', #1410, #1500, #3584 ) ;
#947 = ORIENTED_EDGE ( 'NONE', *, *, #1393, .F. ) ;
#948 = ORIENTED_EDGE ( 'NONE', *, *, #4023, .F. ) ;
#949 = DIRECTION ( 'NONE',  ( -1.000000000000000000, 1.076498916035107744E-16, 0.000000000000000000 ) ) ;
#950 = ADVANCED_FACE ( 'NONE', ( #2758 ), #2378, .T. ) ;
#951 = EDGE_CURVE ( 'NONE', #1336, #230, #3440, .T. ) ;
#952 = VERTEX_POINT ( 'NONE', #2782 ) ;
#953 = CARTESIAN_POINT ( 'NONE',  ( -8.369994990996016071, 6.397500832047212427, 18.40096039353565160 ) ) ;
#954 = LINE ( 'NONE', #553, #1501 ) ;
#955 = AXIS2_PLACEMENT_3D ( 'NONE', #4045, #490, #4449 ) ;
#956 =( NAMED_UNIT ( * ) PLANE_ANGLE_UNIT ( ) SI_UNIT ( $, .RADIAN. ) );
#957 = ADVANCED_FACE ( 'NONE', ( #641 ), #2039, .F. ) ;
#958 = CARTESIAN_POINT ( 'NONE',  ( -13.05597643801425711, -5.804668947475532192, 36.54283959188024511 ) ) ;
#959 = DIRECTION ( 'NONE',  ( 0.000000000000000000, 0.000000000000000000, 1.000000000000000000 ) ) ;
#960 = AXIS2_PLACEMENT_3D ( 'NONE', #2587, #2681, #800 ) ;
#961 = EDGE_CURVE ( 'NONE', #2245, #356, #319, .T. ) ;
#962 = CARTESIAN_POINT ( 'NONE',  ( 14.12144740918446395, -2.180874814963778885, 35.20680156843862108 ) ) ;
#963 = EDGE_CURVE ( 'NONE', #98, #3102, #3083, .T. ) ;
#964 = LINE ( 'NONE', #2425, #1946 ) ;
#965 = DIRECTION ( 'NONE',  ( 0.000000000000000000, 0.000000000000000000, -1.000000000000000000 ) ) ;
#966 = CARTESIAN_POINT ( 'NONE',  ( -12.51136893239551640, 6.899599441734563854, 34.24694080209222591 ) ) ;
#967 = AXIS2_PLACEMENT_3D ( 'NONE', #3873, #2228, #3272 ) ;
#968 = ORIENTED_EDGE ( 'NONE', *, *, #3057, .F. ) ;
#969 = CARTESIAN_POINT ( 'NONE',  ( -9.549434556529077899E-17, -3.249382362871961689E-18, 3.749999999999995559 ) ) ;
#970 = DIRECTION ( 'NONE',  ( 0.000000000000000000, 0.000000000000000000, -1.000000000000000000 ) ) ;
#971 = VERTEX_POINT ( 'NONE', #1412 ) ;
#972 = EDGE_LOOP ( 'NONE', ( #2885, #1987, #262, #4171 ) ) ;
#973 = CYLINDRICAL_SURFACE ( 'NONE', #2794, 3.573749999999999538 ) ;
#974 = VECTOR ( 'NONE', #1575, 1000.000000000000000 ) ;
#975 = VERTEX_POINT ( 'NONE', #3121 ) ;
#976 = CARTESIAN_POINT ( 'NONE',  ( 17.78000050552179800, -17.28000000000000114, 17.28000050552179445 ) ) ;
#977 = FACE_BOUND ( 'NONE', #335, .T. ) ;
#978 = DIRECTION ( 'NONE',  ( -0.000000000000000000, -0.000000000000000000, -1.000000000000000000 ) ) ;
#979 = LINE ( 'NONE', #2086, #4508 ) ;
#980 = CARTESIAN_POINT ( 'NONE',  ( 14.24237576372499170, -1.155158225338516198, 35.75590635509291104 ) ) ;
#981 = CARTESIAN_POINT ( 'NONE',  ( -6.869992765438046156, 6.401597986548673624, 17.15262445358908039 ) ) ;
#982 = EDGE_LOOP ( 'NONE', ( #3300, #3304, #664, #807, #4337 ) ) ;
#983 = CARTESIAN_POINT ( 'NONE',  ( 2.540000505521796015, -10.16000000000000014, 13.73375050552179744 ) ) ;
#984 = CARTESIAN_POINT ( 'NONE',  ( 14.28750723456195537, 0.004097986548674278397, 3.292624453589077405 ) ) ;
#985 = AXIS2_PLACEMENT_3D ( 'NONE', #2268, #3703, #1179 ) ;
#986 = ORIENTED_EDGE ( 'NONE', *, *, #4578, .F. ) ;
#987 = VECTOR ( 'NONE', #1300, 1000.000000000000000 ) ;
#988 = DIRECTION ( 'NONE',  ( -0.000000000000000000, -0.000000000000000000, -1.000000000000000000 ) ) ;
#989 = PRODUCT_DEFINITION_SHAPE ( 'NONE', 'NONE',  #1350 ) ;
#990 = CYLINDRICAL_SURFACE ( 'NONE', #3958, 0.5000000000000004441 ) ;
#991 = ORIENTED_EDGE ( 'NONE', *, *, #2940, .F. ) ;
#992 = VERTEX_POINT ( 'NONE', #3890 ) ;
#993 = EDGE_CURVE ( 'NONE', #3784, #3671, #2297, .T. ) ;
#994 = PRODUCT_RELATED_PRODUCT_CATEGORY ( 'part', '', ( #2403 ) ) ;
#995 = EDGE_CURVE ( 'NONE', #4208, #4575, #3682, .T. ) ;
#996 = EDGE_CURVE ( 'NONE', #1630, #3060, #2107, .T. ) ;
#997 = ORIENTED_EDGE ( 'NONE', *, *, #2321, .F. ) ;
#998 = CARTESIAN_POINT ( 'NONE',  ( 12.37117714425455084, 7.147500832047210650, 18.29228486772272078 ) ) ;
#999 = CARTESIAN_POINT ( 'NONE',  ( -17.48249499099600968, -7.897499167952782173, 18.40096039353565160 ) ) ;
#1000 = CARTESIAN_POINT ( 'NONE',  ( -12.27094482009613685, 7.322808560776099540, 17.41568789468882983 ) ) ;
#1001 = DIRECTION ( 'NONE',  ( 1.000000000000000000, 0.000000000000000000, 0.000000000000000000 ) ) ;
#1002 = CARTESIAN_POINT ( 'NONE',  ( 3.262507234561983438, 0.004097986548672528061, -10.04237554641092345 ) ) ;
#1003 = CARTESIAN_POINT ( 'NONE',  ( -14.17571073093805545, -1.790345610955943467, 28.76824840355960333 ) ) ;
#1004 = CARTESIAN_POINT ( 'NONE',  ( -14.28750000000000142, -3.249382362871961689E-18, 131.2499999999999716 ) ) ;
#1005 = SHAPE_REPRESENTATION ( 'Part 130_Varsay\X2\0131\X0\lan', ( #4483 ), #2891 ) ;
#1006 = DIRECTION ( 'NONE',  ( 1.000000000000000000, 0.000000000000000000, 0.000000000000000000 ) ) ;
#1007 = DIRECTION ( 'NONE',  ( 0.000000000000000000, 0.000000000000000000, 1.000000000000000000 ) ) ;
#1008 = ORIENTED_EDGE ( 'NONE', *, *, #72, .T. ) ;
#1009 = ADVANCED_FACE ( 'NONE', ( #3614 ), #3267, .T. ) ;
#1010 = DIRECTION ( 'NONE',  ( 0.000000000000000000, 0.000000000000000000, 1.000000000000000000 ) ) ;
#1011 = DIRECTION ( 'NONE',  ( -1.000000000000000000, 0.000000000000000000, 0.000000000000000000 ) ) ;
#1012 = DIRECTION ( 'NONE',  ( 1.000000000000000000, 0.000000000000000000, 0.000000000000000000 ) ) ;
#1013 = ADVANCED_FACE ( 'NONE', ( #3237 ), #2230, .T. ) ;
#1014 = EDGE_LOOP ( 'NONE', ( #2060, #2291, #2313, #4100 ) ) ;
#1015 = ORIENTED_EDGE ( 'NONE', *, *, #1490, .T. ) ;
#1016 = ADVANCED_FACE ( 'NONE', ( #68 ), #93, .F. ) ;
#1017 =( NAMED_UNIT ( * ) SI_UNIT ( $, .STERADIAN. ) SOLID_ANGLE_UNIT ( ) );
#1018 = ORIENTED_EDGE ( 'NONE', *, *, #3857, .T. ) ;
#1019 = CARTESIAN_POINT ( 'NONE',  ( -8.369994990996019624, -7.147499167952783061, 18.40096039353565160 ) ) ;
#1020 = ORIENTED_EDGE ( 'NONE', *, *, #3764, .F. ) ;
#1021 = DIRECTION ( 'NONE',  ( 0.000000000000000000, 0.000000000000000000, 1.000000000000000000 ) ) ;
#1022 = CLOSED_SHELL ( 'NONE', ( #2136, #1105, #1564, #950, #893, #3020, #1395, #854, #3469, #3039, #3338, #4640, #2519, #3985 ) ) ;
#1023 = CIRCLE ( 'NONE', #3047, 3.573750000000000426 ) ;
#1024 =( NAMED_UNIT ( * ) SI_UNIT ( $, .STERADIAN. ) SOLID_ANGLE_UNIT ( ) );
#1025 = CARTESIAN_POINT ( 'NONE',  ( 7.234561953626996335E-06, 0.004097986548672528061, -8.542375546410942988 ) ) ;
#1026 = DIRECTION ( 'NONE',  ( -1.000000000000000000, 0.000000000000000000, 0.000000000000000000 ) ) ;
#1027 = LINE ( 'NONE', #1741, #592 ) ;
#1028 = CIRCLE ( 'NONE', #1643, 14.28750000000000142 ) ;
#1029 = DIRECTION ( 'NONE',  ( 1.000000000000000000, 0.000000000000000000, 0.000000000000000000 ) ) ;
#1030 = CARTESIAN_POINT ( 'NONE',  ( 7.234561953626996335E-06, 0.004097986548672528061, 17.16762445358907385 ) ) ;
#1031 = PRODUCT ( 'Part 131_Varsay\X2\0131\X0\lan', 'Part 131_Varsay\X2\0131\X0\lan', '', ( #687 ) ) ;
#1032 = CARTESIAN_POINT ( 'NONE',  ( -12.13219476556017540, -7.546706554720789661, 17.73167833386939307 ) ) ;
#1033 = CARTESIAN_POINT ( 'NONE',  ( 6.586250505521797471, -10.16000000000000014, 13.73375050552179744 ) ) ;
#1034 = AXIS2_PLACEMENT_3D ( 'NONE', #1253, #2668, #887 ) ;
#1035 = LINE ( 'NONE', #3418, #2114 ) ;
#1036 = ORIENTED_EDGE ( 'NONE', *, *, #3500, .T. ) ;
#1037 = CARTESIAN_POINT ( 'NONE',  ( 12.37117936981252164, -7.143402013451326305, 31.86762445358908735 ) ) ;
#1038 = AXIS2_PLACEMENT_3D ( 'NONE', #2839, #1329, #237 ) ;
#1039 = CARTESIAN_POINT ( 'NONE',  ( 2.540000505521796015, -3.039999999999999591, 17.78000050552179445 ) ) ;
#1040 = ORIENTED_EDGE ( 'NONE', *, *, #3222, .F. ) ;
#1041 = ORIENTED_EDGE ( 'NONE', *, *, #2751, .T. ) ;
#1042 = CARTESIAN_POINT ( 'NONE',  ( -12.62991449782762743, 6.684514975176426788, 34.41960495102418349 ) ) ;
#1043 = VECTOR ( 'NONE', #427, 1000.000000000000000 ) ;
#1044 = VERTEX_POINT ( 'NONE', #2905 ) ;
#1045 = DIRECTION ( 'NONE',  ( 1.000000000000000000, -1.076498916035107744E-16, 0.000000000000000000 ) ) ;
#1046 = ORIENTED_EDGE ( 'NONE', *, *, #1699, .F. ) ;
#1047 = B_SPLINE_CURVE_WITH_KNOTS ( 'NONE', 3,
 ( #3336, #1554, #4417, #1205, #156, #2624, #2272, #2196, #1850, #4293 ),
 .UNSPECIFIED., .F., .F.,
 ( 4, 2, 2, 2, 4 ),
 ( 0.000000000000000000, 0.0003199342119934981852, 0.0006398684239869963705, 0.0009598026359804945557, 0.001279736847973992741 ),
 .UNSPECIFIED. ) ;
#1048 = CARTESIAN_POINT ( 'NONE',  ( 17.28000050552179445, -2.539999999999999591, 3.040000505521795571 ) ) ;
#1049 = CARTESIAN_POINT ( 'NONE',  ( 13.83082306713783538, 3.609921861597947590, 38.05633745867911699 ) ) ;
#1050 = CIRCLE ( 'NONE', #3604, 1.499999999999999556 ) ;
#1051 = CARTESIAN_POINT ( 'NONE',  ( 13.86256568255526034, -3.458942830591085205, 31.43753846713071809 ) ) ;
#1052 = LINE ( 'NONE', #642, #2994 ) ;
#1053 = DIRECTION ( 'NONE',  ( 1.000000000000000000, 0.000000000000000000, 0.000000000000000000 ) ) ;
#1054 = CARTESIAN_POINT ( 'NONE',  ( -14.09196727617781164, -2.361570152882583873, 29.67356755769036880 ) ) ;
#1055 = DIRECTION ( 'NONE',  ( 1.000000000000000000, 0.000000000000000000, 0.000000000000000000 ) ) ;
#1056 = CARTESIAN_POINT ( 'NONE',  ( 7.234561953626996335E-06, 0.004097986548672528061, 17.16762445358907385 ) ) ;
#1057 = CARTESIAN_POINT ( 'NONE',  ( 3.573749999999998650, 4.376581498452851814E-16, 4.762500000000001066 ) ) ;
#1058 = LINE ( 'NONE', #4253, #2928 ) ;
#1059 = ORIENTED_EDGE ( 'NONE', *, *, #2895, .T. ) ;
#1060 = CARTESIAN_POINT ( 'NONE',  ( 14.28750723456195360, -0.4767427782355697641, 39.01512445358908820 ) ) ;
#1061 = AXIS2_PLACEMENT_3D ( 'NONE', #346, #2877, #2834 ) ;
#1062 = DIRECTION ( 'NONE',  ( 0.000000000000000000, 1.000000000000000000, 0.000000000000000000 ) ) ;
#1063 = VECTOR ( 'NONE', #852, 1000.000000000000000 ) ;
#1064 = ORIENTED_EDGE ( 'NONE', *, *, #993, .F. ) ;
#1065 = EDGE_LOOP ( 'NONE', ( #1455, #336, #1469 ) ) ;
#1066 = ORIENTED_EDGE ( 'NONE', *, *, #39, .F. ) ;
#1067 = CIRCLE ( 'NONE', #2633, 3.262500000000029932 ) ;
#1068 = CARTESIAN_POINT ( 'NONE',  ( -13.23917829357126585, 5.378272323959379264, 36.58546145169297859 ) ) ;
#1069 = AXIS2_PLACEMENT_3D ( 'NONE', #855, #1198, #2592 ) ;
#1070 = ADVANCED_FACE ( 'NONE', ( #1087 ), #721, .T. ) ;
#1071 = ORIENTED_EDGE ( 'NONE', *, *, #743, .F. ) ;
#1072 = CARTESIAN_POINT ( 'NONE',  ( 11.90639614989969886, 7.897500832047208874, 17.65096039353565160 ) ) ;
#1073 = CARTESIAN_POINT ( 'NONE',  ( -13.92246927997690520, 3.214374465122185942, 30.27987343953798671 ) ) ;
#1074 = AXIS2_PLACEMENT_3D ( 'NONE', #891, #866, #3438 ) ;
#1075 = PRODUCT_CONTEXT ( 'NONE', #1115, 'mechanical' ) ;
#1076 = CARTESIAN_POINT ( 'NONE',  ( -13.11668702015748345, 5.666584765013171321, 36.72824904517413103 ) ) ;
#1077 = LINE ( 'NONE', #2219, #2407 ) ;
#1078 = CARTESIAN_POINT ( 'NONE',  ( 14.20094901052502934, -1.585078670707976922, 29.15451588337786859 ) ) ;
#1079 = LINE ( 'NONE', #35, #4372 ) ;
#1080 = LINE ( 'NONE', #3988, #3239 ) ;
#1081 = DIRECTION ( 'NONE',  ( 0.000000000000000000, 0.000000000000000000, 1.000000000000000000 ) ) ;
#1082 = DIRECTION ( 'NONE',  ( 0.000000000000000000, -1.000000000000000000, 0.000000000000000000 ) ) ;
#1083 = LINE ( 'NONE', #3766, #2773 ) ;
#1084 = ORIENTED_EDGE ( 'NONE', *, *, #747, .T. ) ;
#1085 = DIRECTION ( 'NONE',  ( -1.000000000000000000, 1.076498916035107621E-16, 0.000000000000000000 ) ) ;
#1086 = CIRCLE ( 'NONE', #1167, 0.7500000000000006661 ) ;
#1087 = FACE_OUTER_BOUND ( 'NONE', #1448, .T. ) ;
#1088 = DIRECTION ( 'NONE',  ( 1.000000000000000000, 0.000000000000000000, 0.000000000000000000 ) ) ;
#1089 = ORIENTED_EDGE ( 'NONE', *, *, #4188, .F. ) ;
#1090 = ORIENTED_EDGE ( 'NONE', *, *, #401, .T. ) ;
#1091 = EDGE_CURVE ( 'NONE', #952, #919, #1294, .T. ) ;
#1092 = DIRECTION ( 'NONE',  ( 1.000000000000000000, 0.000000000000000000, 0.000000000000000000 ) ) ;
#1093 = VERTEX_POINT ( 'NONE', #2503 ) ;
#1094 = ORIENTED_EDGE ( 'NONE', *, *, #2618, .T. ) ;
#1095 = CARTESIAN_POINT ( 'NONE',  ( -13.83332089671217346, 3.577847986548673642, 31.63353834203060089 ) ) ;
#1096 = APPLICATION_PROTOCOL_DEFINITION ( 'draft international standard', 'automotive_design', 1998, #324 ) ;
#1097 = LINE ( 'NONE', #3960, #1525 ) ;
#1098 = EDGE_CURVE ( 'NONE', #4620, #1844, #399, .T. ) ;
#1099 = ADVANCED_FACE ( 'NONE', ( #2528 ), #1886, .F. ) ;
#1100 = CARTESIAN_POINT ( 'NONE',  ( 13.42356499362135480, 4.900085295398275420, 37.07996709761046361 ) ) ;
#1101 = DIRECTION ( 'NONE',  ( -0.000000000000000000, 1.000000000000000000, 0.000000000000000000 ) ) ;
#1102 = DIRECTION ( 'NONE',  ( 1.000000000000000000, -0.000000000000000000, -0.000000000000000000 ) ) ;
#1103 = EDGE_CURVE ( 'NONE', #4454, #1942, #2862, .T. ) ;
#1104 = CARTESIAN_POINT ( 'NONE',  ( -3.749994990996019961, -3.749999167952787094, 3.790960393535649064 ) ) ;
#1105 = ADVANCED_FACE ( 'NONE', ( #2603, #376 ), #1819, .F. ) ;
#1106 = FACE_OUTER_BOUND ( 'NONE', #3904, .T. ) ;
#1107 = CIRCLE ( 'NONE', #1710, 3.573750000000000426 ) ;
#1108 = CARTESIAN_POINT ( 'NONE',  ( 13.88012569863659884, -3.384623209710483138, 33.02628322023617358 ) ) ;
#1109 = PRESENTATION_STYLE_ASSIGNMENT (( #4324 ) ) ;
#1110 = CARTESIAN_POINT ( 'NONE',  ( 14.28750723456195537, 0.004097986548674278397, 28.29387445358909403 ) ) ;
#1111 = TOROIDAL_SURFACE ( 'NONE', #572, 1.500000000000000000, 0.7500000000000000000 ) ;
#1112 = EDGE_LOOP ( 'NONE', ( #219, #1218, #682, #4622 ) ) ;
#1113 = CARTESIAN_POINT ( 'NONE',  ( 14.03248876714921778, 2.692596214963125512, 34.72730100679951448 ) ) ;
#1114 = DIRECTION ( 'NONE',  ( 0.000000000000000000, -1.000000000000000000, 0.000000000000000000 ) ) ;
#1115 = APPLICATION_CONTEXT ( 'automotive_design' ) ;
#1116 = B_SPLINE_CURVE_WITH_KNOTS ( 'NONE', 3,
 ( #4017, #351, #4398, #2601, #1489, #397, #1113, #789, #2930, #4327, #3947, #2502, #3221, #720, #2159, #3996 ),
 .UNSPECIFIED., .F., .F.,
 ( 4, 2, 2, 2, 2, 2, 2, 4 ),
 ( 0.01121777374642162449, 0.01261988060185674672, 0.01332093402957430783, 0.01402198745729186895, 0.01472304088500943006, 0.01542409431272699118, 0.01612514774044455229, 0.01682620116816211167 ),
 .UNSPECIFIED. ) ;
#1117 = CARTESIAN_POINT ( 'NONE',  ( 5.009003980371977336E-06, 8.320472128100606877E-07, 3.790960393535649064 ) ) ;
#1118 = AXIS2_PLACEMENT_3D ( 'NONE', #3853, #1689, #3533 ) ;
#1119 = ORIENTED_EDGE ( 'NONE', *, *, #4312, .T. ) ;
#1120 = ORIENTED_EDGE ( 'NONE', *, *, #1171, .T. ) ;
#1121 = DIRECTION ( 'NONE',  ( 0.000000000000000000, 0.000000000000000000, 1.000000000000000000 ) ) ;
#1122 = AXIS2_PLACEMENT_3D ( 'NONE', #3295, #4378, #92 ) ;
#1123 = ORIENTED_EDGE ( 'NONE', *, *, #3319, .T. ) ;
#1124 = CARTESIAN_POINT ( 'NONE',  ( -14.25897937559747675, 0.9352445913789079190, 28.40934117879051257 ) ) ;
#1125 = DIRECTION ( 'NONE',  ( 1.673071420628320689E-16, 0.9999999999999998890, -6.938893903907228378E-18 ) ) ;
#1126 = AXIS2_PLACEMENT_3D ( 'NONE', #4195, #3775, #2419 ) ;
#1127 = CARTESIAN_POINT ( 'NONE',  ( 1.403048712498150108, -3.565902013451326624, -9.476512138277032093 ) ) ;
#1128 = DIRECTION ( 'NONE',  ( -0.000000000000000000, -0.000000000000000000, -1.000000000000000000 ) ) ;
#1129 = EDGE_CURVE ( 'NONE', #4530, #4520, #3688, .T. ) ;
#1130 = CARTESIAN_POINT ( 'NONE',  ( -14.28158997014890375, 0.4709339481348280287, 28.81561122639583417 ) ) ;
#1131 = CARTESIAN_POINT ( 'NONE',  ( -12.30671192345078957, -7.258092364145180220, 17.99507373849870007 ) ) ;
#1132 = VECTOR ( 'NONE', #1533, 1000.000000000000000 ) ;
#1133 = DIRECTION ( 'NONE',  ( 0.000000000000000000, 0.000000000000000000, 1.000000000000000000 ) ) ;
#1134 = CARTESIAN_POINT ( 'NONE',  ( 13.83333536583607781, -3.569652013451328543, 31.86762445358909446 ) ) ;
#1135 = CARTESIAN_POINT ( 'NONE',  ( 3.040000505521796015, -3.039999999999999147, 17.78000050552179445 ) ) ;
#1136 = VECTOR ( 'NONE', #2985, 1000.000000000000000 ) ;
#1137 = ADVANCED_FACE ( 'NONE', ( #1472 ), #3921, .T. ) ;
#1138 = ORIENTED_EDGE ( 'NONE', *, *, #3783, .T. ) ;
#1139 = CARTESIAN_POINT ( 'NONE',  ( 7.620005009003978813, 8.320472119897684647E-07, 32.36596039353566567 ) ) ;
#1140 = CARTESIAN_POINT ( 'NONE',  ( -14.05879861260986630, -2.551382414923340392, 38.54673083970037339 ) ) ;
#1141 = AXIS2_PLACEMENT_3D ( 'NONE', #605, #650, #3847 ) ;
#1142 = DIRECTION ( 'NONE',  ( -1.000000000000000000, 1.076498916035107621E-16, 0.000000000000000000 ) ) ;
#1143 = VERTEX_POINT ( 'NONE', #1233 ) ;
#1144 = ORIENTED_EDGE ( 'NONE', *, *, #1792, .T. ) ;
#1145 = VECTOR ( 'NONE', #4634, 1000.000000000000000 ) ;
#1146 = VECTOR ( 'NONE', #3344, 1000.000000000000000 ) ;
#1147 = ORIENTED_EDGE ( 'NONE', *, *, #1715, .T. ) ;
#1148 = PRODUCT_RELATED_PRODUCT_CATEGORY ( 'part', '', ( #1335 ) ) ;
#1149 = EDGE_LOOP ( 'NONE', ( #3203, #634, #2554, #788 ) ) ;
#1150 = AXIS2_PLACEMENT_3D ( 'NONE', #3611, #2874, #1830 ) ;
#1151 = CARTESIAN_POINT ( 'NONE',  ( 5.009003980371977336E-06, 3.750000832047212906, 3.790960393535649064 ) ) ;
#1152 = EDGE_CURVE ( 'NONE', #2006, #3225, #541, .T. ) ;
#1153 = APPLICATION_PROTOCOL_DEFINITION ( 'draft international standard', 'automotive_design', 1998, #3454 ) ;
#1154 = AXIS2_PLACEMENT_3D ( 'NONE', #1652, #2715, #4156 ) ;
#1155 = CARTESIAN_POINT ( 'NONE',  ( 3.152229664848242852, -3.565902013451327068, -8.542375546410942988 ) ) ;
#1156 = LINE ( 'NONE', #82, #3283 ) ;
#1157 = DIRECTION ( 'NONE',  ( -0.000000000000000000, -0.000000000000000000, -1.000000000000000000 ) ) ;
#1158 = CYLINDRICAL_SURFACE ( 'NONE', #3129, 14.28750000000000142 ) ;
#1159 = CARTESIAN_POINT ( 'NONE',  ( -9.549434556529077899E-17, -3.249382362871961689E-18, 131.2499999999999716 ) ) ;
#1160 = DIRECTION ( 'NONE',  ( -1.076498916035107621E-16, -1.000000000000000000, 0.000000000000000000 ) ) ;
#1161 = CARTESIAN_POINT ( 'NONE',  ( -12.37116490068861019, -7.893402013451320975, 17.15262445358908039 ) ) ;
#1162 = CARTESIAN_POINT ( 'NONE',  ( 7.620005009003977037, 12.08587093932537826, 18.40096039353565160 ) ) ;
#1163 = ORIENTED_EDGE ( 'NONE', *, *, #4168, .F. ) ;
#1164 = CARTESIAN_POINT ( 'NONE',  ( 8.370005009003978813, 6.397500832047211539, 17.65096039353565160 ) ) ;
#1165 = CARTESIAN_POINT ( 'NONE',  ( -13.42355052449745578, -4.891889322300933429, 37.07996709761046361 ) ) ;
#1166 = DIRECTION ( 'NONE',  ( -0.000000000000000000, -0.000000000000000000, -1.000000000000000000 ) ) ;
#1167 = AXIS2_PLACEMENT_3D ( 'NONE', #115, #2979, #2294 ) ;
#1168 = VERTEX_POINT ( 'NONE', #4469 ) ;
#1169 = CARTESIAN_POINT ( 'NONE',  ( 2.540000505521796015, -3.039999999999999591, 17.28000050552179445 ) ) ;
#1170 = CARTESIAN_POINT ( 'NONE',  ( 17.28000050552179445, -3.039999999999999591, 3.040000505521796015 ) ) ;
#1171 = EDGE_CURVE ( 'NONE', #724, #2363, #1982, .T. ) ;
#1172 = DIRECTION ( 'NONE',  ( 0.000000000000000000, 0.000000000000000000, 1.000000000000000000 ) ) ;
#1173 = ORIENTED_EDGE ( 'NONE', *, *, #3501, .T. ) ;
#1174 = EDGE_CURVE ( 'NONE', #4479, #2091, #212, .T. ) ;
#1175 = LINE ( 'NONE', #3082, #1353 ) ;
#1176 = CONTEXT_DEPENDENT_SHAPE_REPRESENTATION ( #2957, #1287 ) ;
#1177 = LINE ( 'NONE', #3013, #3692 ) ;
#1178 = ORIENTED_EDGE ( 'NONE', *, *, #1312, .T. ) ;
#1179 = DIRECTION ( 'NONE',  ( 1.000000000000000000, 0.000000000000000000, -0.000000000000000000 ) ) ;
#1180 = CARTESIAN_POINT ( 'NONE',  ( -3.750000000000000000, 3.750000000000000000, 3.749999999999995559 ) ) ;
#1181 = CARTESIAN_POINT ( 'NONE',  ( -3.750000000000000000, 3.750000000000000000, 3.749999999999995559 ) ) ;
#1182 = CARTESIAN_POINT ( 'NONE',  ( -14.28749276543804569, 0.004097986548671483757, 35.44137445358909133 ) ) ;
#1183 = CARTESIAN_POINT ( 'NONE',  ( 2.540000505521796015, -2.539999999999999591, 2.540000505521796015 ) ) ;
#1184 = CARTESIAN_POINT ( 'NONE',  ( 14.28750000000000142, 1.746464731918909201E-15, 131.2499999999999716 ) ) ;
#1185 = ORIENTED_EDGE ( 'NONE', *, *, #3877, .F. ) ;
#1186 = LINE ( 'NONE', #45, #3815 ) ;
#1187 = CIRCLE ( 'NONE', #119, 0.7500000000000006661 ) ;
#1188 = CARTESIAN_POINT ( 'NONE',  ( -12.76961484722885665, -6.407663495538594489, 35.06035830646955276 ) ) ;
#1189 = ORIENTED_EDGE ( 'NONE', *, *, #951, .F. ) ;
#1190 = CARTESIAN_POINT ( 'NONE',  ( 14.12123733592186348, -2.178197668763618644, 29.02782019034563632 ) ) ;
#1191 = CARTESIAN_POINT ( 'NONE',  ( -12.37116490068861019, 7.151597986548670072, 17.15262445358908039 ) ) ;
#1192 = CARTESIAN_POINT ( 'NONE',  ( -9.549434556529077899E-17, 3.750000000000000000, 131.2499999999999716 ) ) ;
#1193 = VECTOR ( 'NONE', #3110, 1000.000000000000000 ) ;
#1194 = CARTESIAN_POINT ( 'NONE',  ( 17.78000050552179445, -3.039999999999999591, 17.28000050552179445 ) ) ;
#1195 = AXIS2_PLACEMENT_3D ( 'NONE', #2798, #2036, #660 ) ;
#1196 = ORIENTED_EDGE ( 'NONE', *, *, #4290, .F. ) ;
#1197 = CARTESIAN_POINT ( 'NONE',  ( 13.83333314027810701, 3.573750832047210668, 32.36596039353566567 ) ) ;
#1198 = DIRECTION ( 'NONE',  ( 1.000000000000000000, -0.000000000000000000, 0.000000000000000000 ) ) ;
#1199 = AXIS2_PLACEMENT_3D ( 'NONE', #816, #1930, #3731 ) ;
#1200 = ORIENTED_EDGE ( 'NONE', *, *, #1312, .F. ) ;
#1201 = CARTESIAN_POINT ( 'NONE',  ( 12.30672416701672134, 7.262191182741068118, 17.49673779855212885 ) ) ;
#1202 = SHAPE_REPRESENTATION_RELATIONSHIP ( 'NONE' , 'NONE' ,  #1005, #161 ) ;
#1203 = DIRECTION ( 'NONE',  ( -0.000000000000000000, -0.000000000000000000, -1.000000000000000000 ) ) ;
#1204 = CARTESIAN_POINT ( 'NONE',  ( -14.00302738571292593, 2.844081521322073591, 34.04968199708700638 ) ) ;
#1205 = CARTESIAN_POINT ( 'NONE',  ( -12.30737647472887630, 7.256961385541304210, 17.99723211794410460 ) ) ;
#1206 = DIRECTION ( 'NONE',  ( 1.000000000000000000, 0.000000000000000000, 0.000000000000000000 ) ) ;
#1207 =( REPRESENTATION_RELATIONSHIP ('NONE','NONE', #4401, #2003 ) REPRESENTATION_RELATIONSHIP_WITH_TRANSFORMATION ( #79 )SHAPE_REPRESENTATION_RELATIONSHIP( ) );
#1208 = VERTEX_POINT ( 'NONE', #4137 ) ;
#1209 = ADVANCED_FACE ( 'NONE', ( #2652 ), #4498, .F. ) ;
#1210 = PLANE ( 'NONE',  #4039 ) ;
#1211 = CARTESIAN_POINT ( 'NONE',  ( 13.87971749024427304, 3.394489565583088453, 30.71374466332406783 ) ) ;
#1212 = VERTEX_POINT ( 'NONE', #583 ) ;
#1213 = CARTESIAN_POINT ( 'NONE',  ( 13.87988322485530546, -3.385627302013072715, 30.71164830921944500 ) ) ;
#1214 = CARTESIAN_POINT ( 'NONE',  ( 13.73375050552179566, -12.25345428146915161, 6.586250505521797471 ) ) ;
#1215 = LINE ( 'NONE', #1524, #522 ) ;
#1216 = CARTESIAN_POINT ( 'NONE',  ( 14.03249099270719391, 2.696693369464580048, 34.22896506685294327 ) ) ;
#1217 = ORIENTED_EDGE ( 'NONE', *, *, #2893, .F. ) ;
#1218 = ORIENTED_EDGE ( 'NONE', *, *, #741, .T. ) ;
#1219 = CARTESIAN_POINT ( 'NONE',  ( 14.17557912141665888, 1.795475159085173189, 29.26726773362641509 ) ) ;
#1220 = EDGE_CURVE ( 'NONE', #567, #3011, #4443, .T. ) ;
#1221 = B_SPLINE_CURVE_WITH_KNOTS ( 'NONE', 3,
 ( #1072, #1760, #1521, #2801, #2443, #360, #2465, #337, #998, #1805 ),
 .UNSPECIFIED., .F., .F.,
 ( 4, 2, 2, 2, 4 ),
 ( 0.000000000000000000, 0.0003186827706029872194, 0.0006373655412059744388, 0.0009560483118089616039, 0.001274731082411948878 ),
 .UNSPECIFIED. ) ;
#1222 = CIRCLE ( 'NONE', #87, 0.7500000000000006661 ) ;
#1223 = ORIENTED_EDGE ( 'NONE', *, *, #2098, .F. ) ;
#1224 = CARTESIAN_POINT ( 'NONE',  ( 6.586250505521797471, -10.16000000000000014, 6.586250505521798360 ) ) ;
#1225 = PLANE ( 'NONE',  #3529 ) ;
#1226 = CARTESIAN_POINT ( 'NONE',  ( -14.25913809868193383, 0.9325616501008066050, 35.32655817869163428 ) ) ;
#1227 = FACE_OUTER_BOUND ( 'NONE', #2626, .T. ) ;
#1228 = CARTESIAN_POINT ( 'NONE',  ( -3.749994990996019961, -3.749999167952787094, 18.79096039353565217 ) ) ;
#1229 = CIRCLE ( 'NONE', #1453, 3.573749999999999538 ) ;
#1230 = ADVANCED_FACE ( 'NONE', ( #188, #3760 ), #1634, .F. ) ;
#1231 = ORIENTED_EDGE ( 'NONE', *, *, #883, .F. ) ;
#1232 = DIRECTION ( 'NONE',  ( 1.000000000000000000, 0.000000000000000000, -0.000000000000000000 ) ) ;
#1233 = CARTESIAN_POINT ( 'NONE',  ( -11.90638613189173789, 7.897500832047212427, 17.65096039353565160 ) ) ;
#1234 = FACE_OUTER_BOUND ( 'NONE', #2903, .T. ) ;
#1235 = ORIENTED_EDGE ( 'NONE', *, *, #2327, .F. ) ;
#1236 = LINE ( 'NONE', #2656, #1862 ) ;
#1237 = STYLED_ITEM ( 'NONE', ( #244 ), #275 ) ;
#1238 = PRODUCT_DEFINITION_CONTEXT ( 'detailed design', #3989, 'design' ) ;
#1239 = DIRECTION ( 'NONE',  ( 1.000000000000000000, -1.076498916035107621E-16, -0.000000000000000000 ) ) ;
#1240 = EDGE_CURVE ( 'NONE', #4527, #1779, #616, .T. ) ;
#1241 = EDGE_LOOP ( 'NONE', ( #3624, #1709, #1817, #495 ) ) ;
#1242 = ORIENTED_EDGE ( 'NONE', *, *, #280, .F. ) ;
#1243 = FACE_OUTER_BOUND ( 'NONE', #1014, .T. ) ;
#1244 = DIRECTION ( 'NONE',  ( -1.355782318074878530E-16, -1.000000000000000000, 0.000000000000000000 ) ) ;
#1245 = ORIENTED_EDGE ( 'NONE', *, *, #3244, .F. ) ;
#1246 = FACE_OUTER_BOUND ( 'NONE', #3398, .T. ) ;
#1247 = EDGE_CURVE ( 'NONE', #2845, #3903, #920, .T. ) ;
#1248 = CARTESIAN_POINT ( 'NONE',  ( 11.96612007996801630, 7.811560636311104311, 17.15262445358908039 ) ) ;
#1249 = ADVANCED_FACE ( 'NONE', ( #135 ), #488, .T. ) ;
#1250 = DIRECTION ( 'NONE',  ( -8.673617379884035472E-17, -1.000000000000000000, 0.000000000000000000 ) ) ;
#1251 = CARTESIAN_POINT ( 'NONE',  ( 13.11703476964942361, 5.665799994185183763, 36.72925822850186250 ) ) ;
#1252 = DIRECTION ( 'NONE',  ( 0.000000000000000000, 0.000000000000000000, -1.000000000000000000 ) ) ;
#1253 = CARTESIAN_POINT ( 'NONE',  ( 7.620007234561953169, 0.004097986548671708404, 31.86762445358909446 ) ) ;
#1254 = VERTEX_POINT ( 'NONE', #1308 ) ;
#1255 = ADVANCED_FACE ( 'NONE', ( #2721 ), #4164, .T. ) ;
#1256 = CARTESIAN_POINT ( 'NONE',  ( 6.586250505521797471, -10.16000000000000014, 13.73375050552179744 ) ) ;
#1257 = CARTESIAN_POINT ( 'NONE',  ( 14.25899930818333239, 0.9350067622299832459, 28.40931988154160592 ) ) ;
#1258 = AXIS2_PLACEMENT_3D ( 'NONE', #3959, #408, #2892 ) ;
#1259 = ORIENTED_EDGE ( 'NONE', *, *, #2962, .F. ) ;
#1260 = CLOSED_SHELL ( 'NONE', ( #1998, #3537, #1318, #4254 ) ) ;
#1261 = FACE_OUTER_BOUND ( 'NONE', #2120, .T. ) ;
#1262 = ORIENTED_EDGE ( 'NONE', *, *, #3466, .F. ) ;
#1263 = CARTESIAN_POINT ( 'NONE',  ( 6.586250505521797471, -10.16000000000000014, 6.586250505521798360 ) ) ;
#1264 = CARTESIAN_POINT ( 'NONE',  ( 13.92222483456183291, 3.215475260645864086, 33.45288421949413760 ) ) ;
#1265 = ORIENTED_EDGE ( 'NONE', *, *, #2797, .T. ) ;
#1266 = EDGE_LOOP ( 'NONE', ( #2501, #1728, #1991, #2164 ) ) ;
#1267 = LINE ( 'NONE', #1988, #3618 ) ;
#1268 = CIRCLE ( 'NONE', #3880, 0.7499999999999997780 ) ;
#1269 = LINE ( 'NONE', #2686, #1421 ) ;
#1270 = VERTEX_POINT ( 'NONE', #1932 ) ;
#1271 = FACE_BOUND ( 'NONE', #403, .T. ) ;
#1272 = SHAPE_REPRESENTATION_RELATIONSHIP ( 'NONE' , 'NONE' ,  #3415, #2680 ) ;
#1273 = CARTESIAN_POINT ( 'NONE',  ( -3.749994990996019517, 3.750000832047212906, 18.79096039353565217 ) ) ;
#1274 = LINE ( 'NONE', #2693, #2706 ) ;
#1275 = CYLINDRICAL_SURFACE ( 'NONE', #609, 0.7499999999999997780 ) ;
#1276 = EDGE_CURVE ( 'NONE', #1617, #2188, #1580, .T. ) ;
#1277 = ORIENTED_EDGE ( 'NONE', *, *, #1220, .T. ) ;
#1278 = CARTESIAN_POINT ( 'NONE',  ( 12.13299545363123322, -7.541351341831832755, 17.23390984512910507 ) ) ;
#1279 = DIRECTION ( 'NONE',  ( 1.000000000000000000, 0.000000000000000000, 0.000000000000000000 ) ) ;
#1280 = AXIS2_PLACEMENT_3D ( 'NONE', #2732, #31, #2848 ) ;
#1281 = EDGE_CURVE ( 'NONE', #1270, #971, #2811, .T. ) ;
#1282 = B_SPLINE_CURVE_WITH_KNOTS ( 'NONE', 3,
 ( #3720, #2324, #3772, #1646, #3062, #4148, #1547, #2240, #3674, #450, #1898, #3329, #452, #1076, #2493, #2197, #1684, #3104, #4541, #966, #857, #2265, #2991, #4392 ),
 .UNSPECIFIED., .F., .F.,
 ( 4, 2, 2, 2, 2, 2, 2, 2, 2, 2, 2, 4 ),
 ( 8.239936510889833698E-18, 0.001420502804142420540, 0.002841005608284832840, 0.004261508412427245790, 0.004971759814498445326, 0.005682011216569644863, 0.006392262618640844399, 0.007102514020712043935, 0.008523016824854427395, 0.009233268226925630401, 0.009943519628996829937, 0.01136402243313925156 ),
 .UNSPECIFIED. ) ;
#1283 = VERTEX_POINT ( 'NONE', #1057 ) ;
#1284 = CARTESIAN_POINT ( 'NONE',  ( 17.28000050552179800, -17.28000000000000114, 17.78000050552179445 ) ) ;
#1285 = CIRCLE ( 'NONE', #221, 3.573749999999999538 ) ;
#1286 = DIRECTION ( 'NONE',  ( -0.000000000000000000, -0.000000000000000000, -1.000000000000000000 ) ) ;
#1287 = PRODUCT_DEFINITION_SHAPE ( 'NONE', 'NONE',  #4659 ) ;
#1288 = EDGE_LOOP ( 'NONE', ( #4190, #66, #1066, #1381 ) ) ;
#1289 = ORIENTED_EDGE ( 'NONE', *, *, #1933, .T. ) ;
#1290 = PLANE ( 'NONE',  #1678 ) ;
#1291 = DIRECTION ( 'NONE',  ( 0.000000000000000000, -1.000000000000000000, 0.000000000000000000 ) ) ;
#1292 = UNCERTAINTY_MEASURE_WITH_UNIT (LENGTH_MEASURE( 1.000000000000000082E-05 ), #457, 'distance_accuracy_value', 'NONE');
#1293 = ORIENTED_EDGE ( 'NONE', *, *, #1753, .F. ) ;
#1294 = CIRCLE ( 'NONE', #18, 0.7500000000000006661 ) ;
#1295 = LINE ( 'NONE', #3091, #2399 ) ;
#1296 = DIRECTION ( 'NONE',  ( -3.514501480744009400E-17, 1.000000000000000000, 0.000000000000000000 ) ) ;
#1297 = APPLICATION_CONTEXT ( 'automotive_design' ) ;
#1298 = DIRECTION ( 'NONE',  ( 1.000000000000000000, 0.000000000000000000, 0.000000000000000000 ) ) ;
#1299 = CARTESIAN_POINT ( 'NONE',  ( 13.23943158335225334, 5.373578213064656772, 37.08446802545930154 ) ) ;
#1300 = DIRECTION ( 'NONE',  ( 0.000000000000000000, 0.000000000000000000, -1.000000000000000000 ) ) ;
#1301 = CIRCLE ( 'NONE', #3088, 3.262500000000029932 ) ;
#1302 = AXIS2_PLACEMENT_3D ( 'NONE', #4205, #4228, #2090 ) ;
#1303 = EDGE_CURVE ( 'NONE', #2728, #3460, #2764, .T. ) ;
#1304 = CARTESIAN_POINT ( 'NONE',  ( -13.92260559306886236, -3.205595778353110159, 30.27860310428867052 ) ) ;
#1305 = VERTEX_POINT ( 'NONE', #4561 ) ;
#1306 = CARTESIAN_POINT ( 'NONE',  ( 2.540000505521796015, -2.539999999999999591, 17.78000050552179445 ) ) ;
#1307 = AXIS2_PLACEMENT_3D ( 'NONE', #367, #2832, #1812 ) ;
#1308 = CARTESIAN_POINT ( 'NONE',  ( -3.750000000000001776, -3.750000000000000000, 18.74999999999999645 ) ) ;
#1309 = ORIENTED_EDGE ( 'NONE', *, *, #3374, .T. ) ;
#1310 = VECTOR ( 'NONE', #2340, 1000.000000000000000 ) ;
#1311 = CARTESIAN_POINT ( 'NONE',  ( 3.040000505521796015, -3.039999999999999591, 3.040000505521796015 ) ) ;
#1312 = EDGE_CURVE ( 'NONE', #1305, #4255, #1928, .T. ) ;
#1313 = CARTESIAN_POINT ( 'NONE',  ( 17.28000050552179800, -17.28000000000000114, 17.28000050552179445 ) ) ;
#1314 = EDGE_LOOP ( 'NONE', ( #4261, #1144, #4001, #2511, #3951, #2766, #1545, #515, #2165, #2082, #3629, #3382, #4056, #1242, #4569, #1319 ) ) ;
#1315 = EDGE_LOOP ( 'NONE', ( #1633, #2629, #486, #2058 ) ) ;
#1316 = EDGE_CURVE ( 'NONE', #3312, #4530, #3527, .T. ) ;
#1317 = DIRECTION ( 'NONE',  ( -0.000000000000000000, -0.000000000000000000, -1.000000000000000000 ) ) ;
#1318 = ADVANCED_FACE ( 'NONE', ( #2788 ), #1346, .T. ) ;
#1319 = ORIENTED_EDGE ( 'NONE', *, *, #375, .F. ) ;
#1320 = AXIS2_PLACEMENT_3D ( 'NONE', #3949, #3998, #2562 ) ;
#1321 = PLANE ( 'NONE',  #1280 ) ;
#1322 = CARTESIAN_POINT ( 'NONE',  ( -14.12110210206280136, -2.183034303507356277, 35.20514053939854904 ) ) ;
#1323 = CARTESIAN_POINT ( 'NONE',  ( 13.42337887132440066, -4.896491311848273575, 37.57783078324375481 ) ) ;
#1324 = DIRECTION ( 'NONE',  ( 0.000000000000000000, 0.000000000000000000, -1.000000000000000000 ) ) ;
#1325 = CARTESIAN_POINT ( 'NONE',  ( -14.26312271147663502, -0.9396272187553439403, 28.88658383315958389 ) ) ;
#1326 = DIRECTION ( 'NONE',  ( -1.000000000000000000, 1.076498916035107744E-16, 0.000000000000000000 ) ) ;
#1327 = CARTESIAN_POINT ( 'NONE',  ( 17.78000050552179445, -10.16000000000000014, 13.73375050552179744 ) ) ;
#1328 = ORIENTED_EDGE ( 'NONE', *, *, #233, .F. ) ;
#1329 = DIRECTION ( 'NONE',  ( -1.000000000000000000, -0.000000000000000000, 0.000000000000000000 ) ) ;
#1330 = DIRECTION ( 'NONE',  ( 0.000000000000000000, 0.000000000000000000, 1.000000000000000000 ) ) ;
#1331 = AXIS2_PLACEMENT_3D ( 'NONE', #3986, #2195, #33 ) ;
#1332 = VERTEX_POINT ( 'NONE', #2070 ) ;
#1333 = EDGE_CURVE ( 'NONE', #3048, #3625, #4204, .T. ) ;
#1334 = ORIENTED_EDGE ( 'NONE', *, *, #4082, .F. ) ;
#1335 = PRODUCT ( 'Part 136_Varsay\X2\0131\X0\lan', 'Part 136_Varsay\X2\0131\X0\lan', '', ( #2468 ) ) ;
#1336 = VERTEX_POINT ( 'NONE', #2111 ) ;
#1337 = FACE_OUTER_BOUND ( 'NONE', #4167, .T. ) ;
#1338 = DIRECTION ( 'NONE',  ( 2.286980083077370278E-17, -1.000000000000000000, 1.156170392091249751E-18 ) ) ;
#1339 = CARTESIAN_POINT ( 'NONE',  ( -13.23942156534429415, -5.373576548970228295, 37.08446802545930154 ) ) ;
#1340 = CYLINDRICAL_SURFACE ( 'NONE', #3905, 4.762499999999999289 ) ;
#1341 = SURFACE_STYLE_USAGE ( .BOTH. , #3823 ) ;
#1342 = CIRCLE ( 'NONE', #3654, 7.147499999999999076 ) ;
#1343 = DIRECTION ( 'NONE',  ( 1.000000000000000000, 0.000000000000000000, 0.000000000000000000 ) ) ;
#1344 = DIRECTION ( 'NONE',  ( -1.000000000000000000, 8.673617379884035472E-17, 0.000000000000000000 ) ) ;
#1345 = ORIENTED_EDGE ( 'NONE', *, *, #2186, .T. ) ;
#1346 = PLANE ( 'NONE',  #3384 ) ;
#1347 = LINE ( 'NONE', #192, #3912 ) ;
#1348 = AXIS2_PLACEMENT_3D ( 'NONE', #1139, #418, #2883 ) ;
#1349 = EDGE_CURVE ( 'NONE', #3252, #2304, #1397, .T. ) ;
#1350 = PRODUCT_DEFINITION ( 'UNKNOWN', '', #3200, #3391 ) ;
#1351 = VERTEX_POINT ( 'NONE', #983 ) ;
#1352 = DIRECTION ( 'NONE',  ( -1.000000000000000000, 1.076498916035107744E-16, 0.000000000000000000 ) ) ;
#1353 = VECTOR ( 'NONE', #943, 1000.000000000000000 ) ;
#1354 = EDGE_CURVE ( 'NONE', #4402, #1044, #3919, .T. ) ;
#1355 = DIRECTION ( 'NONE',  ( -0.000000000000000000, -0.000000000000000000, -1.000000000000000000 ) ) ;
#1356 = ORIENTED_EDGE ( 'NONE', *, *, #120, .T. ) ;
#1357 = APPLICATION_CONTEXT ( 'automotive_design' ) ;
#1358 = ORIENTED_EDGE ( 'NONE', *, *, #3194, .T. ) ;
#1359 = CARTESIAN_POINT ( 'NONE',  ( -3.750000000000000000, 3.750000000000000000, 18.74999999999999645 ) ) ;
#1360 = VECTOR ( 'NONE', #1429, 1000.000000000000000 ) ;
#1361 = ORIENTED_EDGE ( 'NONE', *, *, #2467, .T. ) ;
#1362 = DIRECTION ( 'NONE',  ( 1.000000000000000000, 0.000000000000000000, 0.000000000000000000 ) ) ;
#1363 = DIRECTION ( 'NONE',  ( -0.000000000000000000, -0.000000000000000000, 1.000000000000000000 ) ) ;
#1364 =( LENGTH_UNIT ( ) NAMED_UNIT ( * ) SI_UNIT ( .MILLI., .METRE. ) );
#1365 = CARTESIAN_POINT ( 'NONE',  ( -14.28749499099602005, 8.320472128100606877E-07, 39.51346039353565942 ) ) ;
#1366 = CARTESIAN_POINT ( 'NONE',  ( 12.76994908703544418, -6.411093920557875414, 35.55968826673669980 ) ) ;
#1367 = DIRECTION ( 'NONE',  ( -0.000000000000000000, -0.000000000000000000, -1.000000000000000000 ) ) ;
#1368 = VECTOR ( 'NONE', #2406, 1000.000000000000000 ) ;
#1369 = EDGE_CURVE ( 'NONE', #1649, #245, #749, .T. ) ;
#1370 = CARTESIAN_POINT ( 'NONE',  ( -14.28749276543805102, -0.4634559803284261648, 28.29387445358910469 ) ) ;
#1371 = CARTESIAN_POINT ( 'NONE',  ( 17.78000050552179445, -10.16000000000000014, 10.16000050552179701 ) ) ;
#1372 = AXIS2_PLACEMENT_3D ( 'NONE', #4346, #1467, #1485 ) ;
#1373 = DIRECTION ( 'NONE',  ( 1.000000000000000000, -0.000000000000000000, 0.000000000000000000 ) ) ;
#1374 = LINE ( 'NONE', #3269, #3161 ) ;
#1375 = EDGE_CURVE ( 'NONE', #3489, #3350, #3759, .T. ) ;
#1376 = EDGE_CURVE ( 'NONE', #1428, #2975, #1743, .T. ) ;
#1377 = VECTOR ( 'NONE', #297, 1000.000000000000000 ) ;
#1378 = ORIENTED_EDGE ( 'NONE', *, *, #1734, .F. ) ;
#1379 = CARTESIAN_POINT ( 'NONE',  ( 13.30085109409153787, -5.216069998034902788, 36.75526953962744159 ) ) ;
#1380 = LINE ( 'NONE', #3831, #1418 ) ;
#1381 = ORIENTED_EDGE ( 'NONE', *, *, #1992, .F. ) ;
#1382 = PRESENTATION_STYLE_ASSIGNMENT (( #3160 ) ) ;
#1383 = ADVANCED_FACE ( 'NONE', ( #2382 ), #3146, .F. ) ;
#1384 = EDGE_LOOP ( 'NONE', ( #4211, #727, #2317, #146 ) ) ;
#1385 = CYLINDRICAL_SURFACE ( 'NONE', #3875, 4.762499999999999289 ) ;
#1386 = EDGE_LOOP ( 'NONE', ( #1800, #3090, #991, #200 ) ) ;
#1387 = CYLINDRICAL_SURFACE ( 'NONE', #4119, 0.5000000000000004441 ) ;
#1388 = DIRECTION ( 'NONE',  ( 6.017322057294549609E-18, 0.000000000000000000, -1.000000000000000000 ) ) ;
#1389 = FACE_OUTER_BOUND ( 'NONE', #1527, .T. ) ;
#1390 = DIRECTION ( 'NONE',  ( 0.000000000000000000, 0.000000000000000000, -1.000000000000000000 ) ) ;
#1391 = DIRECTION ( 'NONE',  ( -1.000000000000000000, -0.000000000000000000, -0.000000000000000000 ) ) ;
#1392 = AXIS2_PLACEMENT_3D ( 'NONE', #366, #2852, #3234 ) ;
#1393 = EDGE_CURVE ( 'NONE', #3850, #254, #2923, .T. ) ;
#1394 = CARTESIAN_POINT ( 'NONE',  ( 13.92261115689014694, -3.209696657368923400, 33.95459613213026984 ) ) ;
#1395 = ADVANCED_FACE ( 'NONE', ( #274 ), #4632, .F. ) ;
#1396 = CARTESIAN_POINT ( 'NONE',  ( 7.620007234561954057, -6.393402013451326305, 31.86762445358908735 ) ) ;
#1397 = LINE ( 'NONE', #628, #301 ) ;
#1398 = LINE ( 'NONE', #2837, #2710 ) ;
#1399 = EDGE_LOOP ( 'NONE', ( #3181, #1941, #3245, #2347, #489, #3507, #2286, #4314, #997, #1690, #138, #1289 ) ) ;
#1400 = CARTESIAN_POINT ( 'NONE',  ( 13.11669926372341344, -5.662485946417288751, 36.22991310522755981 ) ) ;
#1401 = B_SPLINE_CURVE_WITH_KNOTS ( 'NONE', 3,
 ( #697, #1060, #1754, #4544, #3178, #4614, #4637, #4566, #3130, #4209, #3554, #1379, #278, #1400, #2482, #4187, #2074, #2815, #3830, #4279, #4256, #676, #1688, #1037 ),
 .UNSPECIFIED., .F., .F.,
 ( 4, 2, 2, 2, 2, 2, 2, 2, 2, 2, 2, 4 ),
 ( 0.01136174788562027173, 0.01278160237203083797, 0.01420145685844140422, 0.01562131134485196873, 0.01633123858805725359, 0.01704116583126253498, 0.01775109307446781637, 0.01846102031767310123, 0.01988087480408368135, 0.02059080204728896968, 0.02130072929049425801, 0.02272058377690481731 ),
 .UNSPECIFIED. ) ;
#1402 = DIRECTION ( 'NONE',  ( 0.000000000000000000, 0.000000000000000000, 1.000000000000000000 ) ) ;
#1403 = ORIENTED_EDGE ( 'NONE', *, *, #3980, .F. ) ;
#1404 = ORIENTED_EDGE ( 'NONE', *, *, #448, .T. ) ;
#1405 = FILL_AREA_STYLE_COLOUR ( '', #1957 ) ;
#1406 = ORIENTED_EDGE ( 'NONE', *, *, #3488, .F. ) ;
#1407 = CYLINDRICAL_SURFACE ( 'NONE', #3652, 0.5000000000000004441 ) ;
#1408 = VERTEX_POINT ( 'NONE', #4274 ) ;
#1409 = FACE_OUTER_BOUND ( 'NONE', #4356, .T. ) ;
#1410 = CARTESIAN_POINT ( 'NONE',  ( -8.423108025121072373, -11.35554107275920543, -113.4690396064643636 ) ) ;
#1411 = CARTESIAN_POINT ( 'NONE',  ( -14.28749499099602005, -0.4809632029028111933, 39.51346039353565232 ) ) ;
#1412 = CARTESIAN_POINT ( 'NONE',  ( 7.620007234561954057, -6.393402013451325416, 17.90262445358908039 ) ) ;
#1413 = CARTESIAN_POINT ( 'NONE',  ( 8.370005009003978813, 6.397500832047211539, 18.40096039353565160 ) ) ;
#1414 = AXIS2_PLACEMENT_3D ( 'NONE', #663, #3886, #4287 ) ;
#1415 = CARTESIAN_POINT ( 'NONE',  ( -14.03274346603649647, -2.691220199277232883, 30.00305411948872703 ) ) ;
#1416 = DIRECTION ( 'NONE',  ( -1.000000000000000000, 0.000000000000000000, 0.000000000000000000 ) ) ;
#1417 = CARTESIAN_POINT ( 'NONE',  ( 3.750000000000000000, 3.750000000000000000, 146.2500000000000000 ) ) ;
#1418 = VECTOR ( 'NONE', #1355, 1000.000000000000000 ) ;
#1419 = DIRECTION ( 'NONE',  ( 0.000000000000000000, 0.000000000000000000, -1.000000000000000000 ) ) ;
#1420 = B_SPLINE_CURVE_WITH_KNOTS ( 'NONE', 3,
 ( #3878, #1511, #3243, #415, #3270, #1861, #3969, #4396, #19, #1535 ),
 .UNSPECIFIED., .F., .F.,
 ( 4, 2, 2, 2, 4 ),
 ( 0.000000000000000000, 0.0003199342119934985105, 0.0006398684239869970210, 0.0009598026359804955315, 0.001279736847973994042 ),
 .UNSPECIFIED. ) ;
#1421 = VECTOR ( 'NONE', #2709, 1000.000000000000000 ) ;
#1422 = EDGE_LOOP ( 'NONE', ( #2723, #2332, #3770, #766 ) ) ;
#1423 = CARTESIAN_POINT ( 'NONE',  ( 17.78000050552179445, -3.039999999999999591, 3.040000505521795571 ) ) ;
#1424 = EDGE_CURVE ( 'NONE', #2966, #3364, #2477, .T. ) ;
#1425 = AXIS2_PLACEMENT_3D ( 'NONE', #3572, #22, #1470 ) ;
#1426 = CARTESIAN_POINT ( 'NONE',  ( 17.28000050552179800, -17.28000000000000114, 3.040000505521795571 ) ) ;
#1427 = EDGE_LOOP ( 'NONE', ( #4075, #4081, #986, #3437, #4420, #723, #3100, #3832, #4212, #4478, #3643, #4231, #3504, #2488, #1064, #3714 ) ) ;
#1428 = VERTEX_POINT ( 'NONE', #3828 ) ;
#1429 = DIRECTION ( 'NONE',  ( -0.000000000000000000, -0.000000000000000000, -1.000000000000000000 ) ) ;
#1430 = EDGE_LOOP ( 'NONE', ( #1309, #1008, #2741, #3697 ) ) ;
#1431 = DIRECTION ( 'NONE',  ( 0.000000000000000000, 1.000000000000000000, 0.000000000000000000 ) ) ;
#1432 = ORIENTED_EDGE ( 'NONE', *, *, #2584, .F. ) ;
#1433 = LINE ( 'NONE', #3562, #285 ) ;
#1434 = SHAPE_DEFINITION_REPRESENTATION ( #2441, #1824 ) ;
#1435 = VECTOR ( 'NONE', #3406, 1000.000000000000000 ) ;
#1436 = CARTESIAN_POINT ( 'NONE',  ( 17.78000050552179445, -3.039999999999999591, 2.540000505521796015 ) ) ;
#1437 = LINE ( 'NONE', #1878, #4025 ) ;
#1438 = CARTESIAN_POINT ( 'NONE',  ( 10.16000050552179701, -10.16000000000000014, 2.540000505521796015 ) ) ;
#1439 = CYLINDRICAL_SURFACE ( 'NONE', #1302, 3.573749999999999538 ) ;
#1440 = EDGE_CURVE ( 'NONE', #1093, #1498, #2548, .T. ) ;
#1441 = ORIENTED_EDGE ( 'NONE', *, *, #1240, .F. ) ;
#1442 = PLANE ( 'NONE',  #1122 ) ;
#1443 = CARTESIAN_POINT ( 'NONE',  ( 12.39927133462508912, 7.103558341128515252, 32.81963905935650416 ) ) ;
#1444 = AXIS2_PLACEMENT_3D ( 'NONE', #4245, #978, #1026 ) ;
#1445 = CYLINDRICAL_SURFACE ( 'NONE', #930, 0.7500000000000006661 ) ;
#1446 = DIRECTION ( 'NONE',  ( 0.000000000000000000, 0.000000000000000000, -1.000000000000000000 ) ) ;
#1447 = ADVANCED_FACE ( 'NONE', ( #1814 ), #2106, .F. ) ;
#1448 = EDGE_LOOP ( 'NONE', ( #2124, #3685, #551, #2099 ) ) ;
#1449 = EDGE_CURVE ( 'NONE', #4040, #3180, #4344, .T. ) ;
#1450 = VERTEX_POINT ( 'NONE', #86 ) ;
#1451 = CARTESIAN_POINT ( 'NONE',  ( -12.87886805896745201, 6.196644199065969971, 35.46669787887593372 ) ) ;
#1452 =( BOUNDED_CURVE ( )  B_SPLINE_CURVE ( 3, ( #3043, #2623, #3095, #3456 ),
 .UNSPECIFIED., .F., .T. ) 
 B_SPLINE_CURVE_WITH_KNOTS ( ( 4, 4 ),
 ( 3.141592653589793116, 4.712388980384689674 ),
 .UNSPECIFIED. ) 
 CURVE ( )  GEOMETRIC_REPRESENTATION_ITEM ( )  RATIONAL_B_SPLINE_CURVE ( ( 1.000000000000000000, 0.8047378541243649375, 0.8047378541243649375, 1.000000000000000000 ) ) 
 REPRESENTATION_ITEM ( '' )  );
#1453 = AXIS2_PLACEMENT_3D ( 'NONE', #4055, #1648, #3722 ) ;
#1454 = ADVANCED_FACE ( 'NONE', ( #2154 ), #15, .F. ) ;
#1455 = ORIENTED_EDGE ( 'NONE', *, *, #424, .T. ) ;
#1456 = ORIENTED_EDGE ( 'NONE', *, *, #3709, .F. ) ;
#1457 = DIRECTION ( 'NONE',  ( 1.000000000000000000, 0.000000000000000000, 0.000000000000000000 ) ) ;
#1458 = AXIS2_PLACEMENT_3D ( 'NONE', #2978, #4519, #3712 ) ;
#1459 = CARTESIAN_POINT ( 'NONE',  ( -8.427206011669747809, 3.330716161802742992, -145.3366640600534652 ) ) ;
#1460 = CARTESIAN_POINT ( 'NONE',  ( 13.05598868158019066, 5.808767766071424532, 36.04450365193367389 ) ) ;
#1461 = CARTESIAN_POINT ( 'NONE',  ( 14.28750500900398279, -0.2342234701874567893, 28.79221039353567235 ) ) ;
#1462 = DIRECTION ( 'NONE',  ( 0.000000000000000000, 0.000000000000000000, 1.000000000000000000 ) ) ;
#1463 = DIRECTION ( 'NONE',  ( 1.000000000000000000, -1.076498916035107744E-16, -0.000000000000000000 ) ) ;
#1464 = CARTESIAN_POINT ( 'NONE',  ( 13.73375050552179744, -10.16000000000000014, 17.78000050552179445 ) ) ;
#1465 = CARTESIAN_POINT ( 'NONE',  ( 14.28750500900398279, 8.320472145597748469E-07, 28.79221039353566880 ) ) ;
#1466 = CARTESIAN_POINT ( 'NONE',  ( 14.99250500900398109, 7.897500832047208874, 18.40096039353565160 ) ) ;
#1467 = DIRECTION ( 'NONE',  ( 1.076498916035107621E-16, 1.000000000000000000, -0.000000000000000000 ) ) ;
#1468 = LINE ( 'NONE', #1162, #49 ) ;
#1469 = ORIENTED_EDGE ( 'NONE', *, *, #3883, .F. ) ;
#1470 = DIRECTION ( 'NONE',  ( 0.000000000000000000, 1.000000000000000000, 0.000000000000000000 ) ) ;
#1471 = CIRCLE ( 'NONE', #4088, 0.5000000000000000000 ) ;
#1472 = FACE_OUTER_BOUND ( 'NONE', #176, .T. ) ;
#1473 = DIRECTION ( 'NONE',  ( -1.707404996040164265E-16, 1.000000000000000000, 0.000000000000000000 ) ) ;
#1474 = ORIENTED_EDGE ( 'NONE', *, *, #601, .T. ) ;
#1475 = ORIENTED_EDGE ( 'NONE', *, *, #4216, .F. ) ;
#1476 = CARTESIAN_POINT ( 'NONE',  ( -12.37116490068861019, 7.151597986548673624, 32.34872277302695665 ) ) ;
#1477 = ORIENTED_EDGE ( 'NONE', *, *, #2401, .T. ) ;
#1478 = DIRECTION ( 'NONE',  ( 1.076498916035107621E-16, 1.000000000000000000, -0.000000000000000000 ) ) ;
#1479 = DIRECTION ( 'NONE',  ( -1.000000000000000000, 1.661934922188931704E-16, 4.999591919805462731E-18 ) ) ;
#1480 = CARTESIAN_POINT ( 'NONE',  ( 0.5742288748238882912, -3.565902013451327512, -9.691754032660345075 ) ) ;
#1481 = LINE ( 'NONE', #646, #1897 ) ;
#1482 = CARTESIAN_POINT ( 'NONE',  ( -14.09217544079672280, 2.360382569825107968, 29.67243804805142204 ) ) ;
#1483 = DIRECTION ( 'NONE',  ( 1.000000000000000000, 0.000000000000000000, 0.000000000000000000 ) ) ;
#1484 = PLANE ( 'NONE',  #2772 ) ;
#1485 = DIRECTION ( 'NONE',  ( -1.000000000000000000, 0.000000000000000000, 0.000000000000000000 ) ) ;
#1486 = CARTESIAN_POINT ( 'NONE',  ( 3.040000505521796015, -2.539999999999999591, 17.78000050552179445 ) ) ;
#1487 = AXIS2_PLACEMENT_3D ( 'NONE', #4545, #1330, #217 ) ;
#1488 = VERTEX_POINT ( 'NONE', #3635 ) ;
#1489 = CARTESIAN_POINT ( 'NONE',  ( 13.94789236355132545, 3.099469737325899032, 34.16023755992365096 ) ) ;
#1490 = EDGE_CURVE ( 'NONE', #2026, #1270, #149, .T. ) ;
#1491 = CARTESIAN_POINT ( 'NONE',  ( -3.262492765438076869, 0.004097986548672927914, -10.04237554641092345 ) ) ;
#1492 = ADVANCED_FACE ( 'NONE', ( #2922, #738 ), #1484, .F. ) ;
#1493 = ORIENTED_EDGE ( 'NONE', *, *, #606, .F. ) ;
#1494 = ORIENTED_EDGE ( 'NONE', *, *, #2900, .T. ) ;
#1495 = ADVANCED_FACE ( 'NONE', ( #2878, #3966 ), #2522, .F. ) ;
#1496 = SURFACE_STYLE_USAGE ( .BOTH. , #52 ) ;
#1497 = VERTEX_POINT ( 'NONE', #2901 ) ;
#1498 = VERTEX_POINT ( 'NONE', #2203 ) ;
#1499 = CARTESIAN_POINT ( 'NONE',  ( -14.28159601362361286, 0.4702588884268389391, 35.91633004324798861 ) ) ;
#1500 = DIRECTION ( 'NONE',  ( -2.428612866367492338E-17, 1.000000000000000000, 0.000000000000000000 ) ) ;
#1501 = VECTOR ( 'NONE', #289, 1000.000000000000000 ) ;
#1502 = CARTESIAN_POINT ( 'NONE',  ( 13.23943380891023480, 5.377675367566115305, 36.58613208551275164 ) ) ;
#1503 = CARTESIAN_POINT ( 'NONE',  ( 14.09194676216336362, -2.361710026607503288, 29.67376555440869268 ) ) ;
#1504 = CARTESIAN_POINT ( 'NONE',  ( -14.20092530083940296, 1.585302497639503372, 29.15456951301168331 ) ) ;
#1505 = DIRECTION ( 'NONE',  ( 0.000000000000000000, 0.000000000000000000, 1.000000000000000000 ) ) ;
#1506 = CIRCLE ( 'NONE', #4125, 0.7500000000000006661 ) ;
#1507 = FACE_BOUND ( 'NONE', #1149, .T. ) ;
#1508 = EDGE_CURVE ( 'NONE', #2857, #1044, #1285, .T. ) ;
#1509 = CARTESIAN_POINT ( 'NONE',  ( 14.03294734829104051, -2.686071323426693525, 34.23161090455447209 ) ) ;
#1510 = DIRECTION ( 'NONE',  ( 0.000000000000000000, -0.000000000000000000, 1.000000000000000000 ) ) ;
#1511 = CARTESIAN_POINT ( 'NONE',  ( 12.37117714425454551, -7.147499167952783949, 18.29267992112417929 ) ) ;
#1512 = CIRCLE ( 'NONE', #3154, 3.573749999999999538 ) ;
#1513 = VERTEX_POINT ( 'NONE', #3991 ) ;
#1514 = CARTESIAN_POINT ( 'NONE',  ( -3.749999999999999556, 3.750000000000000000, 131.2499999999999716 ) ) ;
#1515 = CARTESIAN_POINT ( 'NONE',  ( 8.370005009003978813, -6.397499167952784838, 3.790960393535648176 ) ) ;
#1516 = EDGE_CURVE ( 'NONE', #657, #1093, #1050, .T. ) ;
#1517 = ADVANCED_FACE ( 'NONE', ( #2947 ), #2499, .F. ) ;
#1518 = AXIS2_PLACEMENT_3D ( 'NONE', #1789, #1082, #1446 ) ;
#1519 = DIRECTION ( 'NONE',  ( -1.355782318074878530E-16, 1.000000000000000000, 0.000000000000000000 ) ) ;
#1520 = ORIENTED_EDGE ( 'NONE', *, *, #2887, .T. ) ;
#1521 = CARTESIAN_POINT ( 'NONE',  ( 12.02320160177486486, 7.719185208846096380, 17.66665972527255235 ) ) ;
#1522 = DIRECTION ( 'NONE',  ( 0.000000000000000000, 0.000000000000000000, 1.000000000000000000 ) ) ;
#1523 = CIRCLE ( 'NONE', #4139, 3.573749999999999538 ) ;
#1524 = CARTESIAN_POINT ( 'NONE',  ( 12.37117936981252164, -7.143402013451325416, 17.15262445358908039 ) ) ;
#1525 = VECTOR ( 'NONE', #4008, 1000.000000000000000 ) ;
#1526 = ORIENTED_EDGE ( 'NONE', *, *, #3586, .F. ) ;
#1527 = EDGE_LOOP ( 'NONE', ( #3204, #2534, #4147, #1591 ) ) ;
#1528 = COLOUR_RGB ( '', 0.09019608, 0.27058824, 0.51372549) ;
#1529 = CARTESIAN_POINT ( 'NONE',  ( -14.25914032423990818, 0.9284644955993464066, 35.82489411863820550 ) ) ;
#1530 = CONTEXT_DEPENDENT_SHAPE_REPRESENTATION ( #1207, #189 ) ;
#1531 = ORIENTED_EDGE ( 'NONE', *, *, #3244, .T. ) ;
#1532 = DIRECTION ( 'NONE',  ( -1.000000000000000000, 1.076498916035107744E-16, 0.000000000000000000 ) ) ;
#1533 = DIRECTION ( 'NONE',  ( -1.000000000000000000, 1.076498916035107744E-16, 0.000000000000000000 ) ) ;
#1534 = CARTESIAN_POINT ( 'NONE',  ( 14.20084427493783430, -1.582011882117793089, 35.07860273982173993 ) ) ;
#1535 = CARTESIAN_POINT ( 'NONE',  ( 11.90639614989970063, -7.897499167952783949, 17.65096039353565160 ) ) ;
#1536 = APPLICATION_CONTEXT ( 'automotive_design' ) ;
#1537 = ADVANCED_FACE ( 'NONE', ( #1106 ), #2096, .F. ) ;
#1538 = ORIENTED_EDGE ( 'NONE', *, *, #3906, .T. ) ;
#1539 = CARTESIAN_POINT ( 'NONE',  ( 3.750005009003979595, 3.750000832047212906, 3.790960393535649064 ) ) ;
#1540 = DIRECTION ( 'NONE',  ( 0.000000000000000000, 1.000000000000000000, 0.000000000000000000 ) ) ;
#1541 = EDGE_LOOP ( 'NONE', ( #1356, #2889, #184, #1245 ) ) ;
#1542 = DIRECTION ( 'NONE',  ( -1.000000000000000000, 0.000000000000000000, 0.000000000000000000 ) ) ;
#1543 = CARTESIAN_POINT ( 'NONE',  ( 5.009003980371977336E-06, 8.320472128100606877E-07, 17.65096039353565160 ) ) ;
#1544 = CARTESIAN_POINT ( 'NONE',  ( 3.040000505521796015, -17.28000000000000114, 3.040000505521795571 ) ) ;
#1545 = ORIENTED_EDGE ( 'NONE', *, *, #2855, .F. ) ;
#1546 = EDGE_LOOP ( 'NONE', ( #4103, #190, #1578 ) ) ;
#1547 = CARTESIAN_POINT ( 'NONE',  ( -13.83078033805465878, 3.606002719002763257, 38.55461960823348022 ) ) ;
#1548 = PRODUCT_RELATED_PRODUCT_CATEGORY ( 'part', '', ( #3876 ) ) ;
#1549 = ORIENTED_EDGE ( 'NONE', *, *, #4501, .F. ) ;
#1550 = LINE ( 'NONE', #4487, #1751 ) ;
#1551 = FACE_OUTER_BOUND ( 'NONE', #3514, .T. ) ;
#1552 = CYLINDRICAL_SURFACE ( 'NONE', #2314, 7.147499999999999076 ) ;
#1553 = CARTESIAN_POINT ( 'NONE',  ( 14.12144963474243298, -2.176777660462316799, 34.70846562849202144 ) ) ;
#1554 = CARTESIAN_POINT ( 'NONE',  ( -12.37116712624658277, 7.147500832047212427, 18.29267992112417929 ) ) ;
#1555 = DIRECTION ( 'NONE',  ( 0.000000000000000000, 1.000000000000000000, 0.000000000000000000 ) ) ;
#1556 = AXIS2_PLACEMENT_3D ( 'NONE', #2734, #1296, #2804 ) ;
#1557 = ORIENTED_EDGE ( 'NONE', *, *, #2983, .F. ) ;
#1558 = CARTESIAN_POINT ( 'NONE',  ( 8.370007234561949616, -7.893402013451326305, 17.15262445358908039 ) ) ;
#1559 = CIRCLE ( 'NONE', #3575, 1.499999999999999556 ) ;
#1560 = CARTESIAN_POINT ( 'NONE',  ( -13.60390977449484318, -4.366406831334375127, 37.52789170789247208 ) ) ;
#1561 = ORIENTED_EDGE ( 'NONE', *, *, #2866, .F. ) ;
#1562 = CARTESIAN_POINT ( 'NONE',  ( 10.16000050552179701, -6.586249999999999716, 10.16000050552179701 ) ) ;
#1563 = AXIS2_PLACEMENT_3D ( 'NONE', #3066, #594, #1672 ) ;
#1564 = ADVANCED_FACE ( 'NONE', ( #3268, #1507 ), #4371, .T. ) ;
#1565 = CARTESIAN_POINT ( 'NONE',  ( 10.16000050552179701, -13.73374999999999879, 10.16000050552179701 ) ) ;
#1566 = DIRECTION ( 'NONE',  ( -0.000000000000000000, -0.000000000000000000, 1.000000000000000000 ) ) ;
#1567 = CARTESIAN_POINT ( 'NONE',  ( 7.620007234561953169, 0.004097986548671547075, 31.86762445358908735 ) ) ;
#1568 = ORIENTED_EDGE ( 'NONE', *, *, #4582, .F. ) ;
#1569 = VERTEX_POINT ( 'NONE', #2223 ) ;
#1570 = CARTESIAN_POINT ( 'NONE',  ( 7.620005009003978813, -3.573749167952787520, 32.36596039353566567 ) ) ;
#1571 = AXIS2_PLACEMENT_3D ( 'NONE', #1705, #3467, #2054 ) ;
#1572 = EDGE_LOOP ( 'NONE', ( #150, #1682, #4239, #3493 ) ) ;
#1573 = FACE_OUTER_BOUND ( 'NONE', #1541, .T. ) ;
#1574 =( NAMED_UNIT ( * ) SI_UNIT ( $, .STERADIAN. ) SOLID_ANGLE_UNIT ( ) );
#1575 = DIRECTION ( 'NONE',  ( -0.000000000000000000, -0.000000000000000000, -1.000000000000000000 ) ) ;
#1576 = CARTESIAN_POINT ( 'NONE',  ( -13.92217699914708895, 3.215616030937979541, 33.45254891481317117 ) ) ;
#1577 = FACE_OUTER_BOUND ( 'NONE', #3371, .T. ) ;
#1578 = ORIENTED_EDGE ( 'NONE', *, *, #3298, .F. ) ;
#1579 = LINE ( 'NONE', #487, #3590 ) ;
#1580 = LINE ( 'NONE', #2426, #3695 ) ;
#1581 = STYLED_ITEM ( 'NONE', ( #357 ), #391 ) ;
#1582 = EDGE_CURVE ( 'NONE', #2669, #4497, #3659, .T. ) ;
#1583 = AXIS2_PLACEMENT_3D ( 'NONE', #1159, #4013, #783 ) ;
#1584 = ORIENTED_EDGE ( 'NONE', *, *, #84, .F. ) ;
#1585 = CARTESIAN_POINT ( 'NONE',  ( 6.870005009003977925, 6.397500832047211539, 18.40096039353565160 ) ) ;
#1586 = CARTESIAN_POINT ( 'NONE',  ( 8.370007234561949616, 7.151597986548671848, 17.90262445358908039 ) ) ;
#1587 = DIRECTION ( 'NONE',  ( 0.000000000000000000, 0.000000000000000000, -1.000000000000000000 ) ) ;
#1588 = CARTESIAN_POINT ( 'NONE',  ( 14.12152400421957132, 2.184333436165076137, 34.70878884231233030 ) ) ;
#1589 = EDGE_CURVE ( 'NONE', #501, #2642, #4394, .T. ) ;
#1590 = EDGE_CURVE ( 'NONE', #2828, #724, #811, .T. ) ;
#1591 = ORIENTED_EDGE ( 'NONE', *, *, #3150, .T. ) ;
#1592 = VERTEX_POINT ( 'NONE', #4489 ) ;
#1593 = CARTESIAN_POINT ( 'NONE',  ( 13.94792677495786570, 3.099290160580272069, 30.57149645866954657 ) ) ;
#1594 = CARTESIAN_POINT ( 'NONE',  ( 17.28000050552179800, -17.28000000000000114, 17.28000050552179445 ) ) ;
#1595 = ADVANCED_FACE ( 'NONE', ( #3680 ), #4415, .F. ) ;
#1596 = ADVANCED_FACE ( 'NONE', ( #4463 ), #1225, .F. ) ;
#1597 = AXIS2_PLACEMENT_3D ( 'NONE', #2350, #931, #909 ) ;
#1598 = ORIENTED_EDGE ( 'NONE', *, *, #1171, .F. ) ;
#1599 = CIRCLE ( 'NONE', #1891, 0.5000000000000004441 ) ;
#1600 = DIRECTION ( 'NONE',  ( 0.000000000000000000, 1.000000000000000000, 0.000000000000000000 ) ) ;
#1601 = PLANE ( 'NONE',  #1782 ) ;
#1602 = DIRECTION ( 'NONE',  ( -1.000000000000000000, 0.000000000000000000, 0.000000000000000000 ) ) ;
#1603 = CARTESIAN_POINT ( 'NONE',  ( 14.99250723456195544, 7.151597986548670072, 31.86762445358908735 ) ) ;
#1604 = CARTESIAN_POINT ( 'NONE',  ( -7.619992765438044380, 6.401597986548673624, 17.90262445358908039 ) ) ;
#1605 = ORIENTED_EDGE ( 'NONE', *, *, #2075, .F. ) ;
#1606 = FACE_OUTER_BOUND ( 'NONE', #3085, .T. ) ;
#1607 = CARTESIAN_POINT ( 'NONE',  ( 13.92220696890103504, 3.215556595662160788, 30.28246602885027983 ) ) ;
#1608 = CARTESIAN_POINT ( 'NONE',  ( -11.90638390633376531, 7.901597986548672736, 17.15262445358908039 ) ) ;
#1609 = ORIENTED_EDGE ( 'NONE', *, *, #4619, .T. ) ;
#1610 = CARTESIAN_POINT ( 'NONE',  ( -8.369994990996019624, -6.397499167952784838, 17.65096039353565160 ) ) ;
#1611 = FACE_OUTER_BOUND ( 'NONE', #1911, .T. ) ;
#1612 = DIRECTION ( 'NONE',  ( -1.000000000000000000, 0.000000000000000000, 0.000000000000000000 ) ) ;
#1613 = PRODUCT_DEFINITION_CONTEXT ( 'detailed design', #2779, 'design' ) ;
#1614 = DIRECTION ( 'NONE',  ( -0.000000000000000000, -1.000000000000000000, -0.000000000000000000 ) ) ;
#1615 = CARTESIAN_POINT ( 'NONE',  ( 17.28000050552179445, -2.539999999999996927, 17.78000050552179445 ) ) ;
#1616 = ORIENTED_EDGE ( 'NONE', *, *, #542, .T. ) ;
#1617 = VERTEX_POINT ( 'NONE', #1995 ) ;
#1618 = ITEM_DEFINED_TRANSFORMATION ( 'NONE', 'NONE', #1556,  #4483 ) ;
#1619 = DIRECTION ( 'NONE',  ( -0.000000000000000000, -0.000000000000000000, 1.000000000000000000 ) ) ;
#1620 = DIRECTION ( 'NONE',  ( 1.000000000000000000, -0.000000000000000000, 0.000000000000000000 ) ) ;
#1621 = EDGE_CURVE ( 'NONE', #4543, #3471, #2995, .T. ) ;
#1622 = UNCERTAINTY_MEASURE_WITH_UNIT (LENGTH_MEASURE( 1.000000000000000082E-05 ), #4035, 'distance_accuracy_value', 'NONE');
#1623 = VERTEX_POINT ( 'NONE', #1626 ) ;
#1624 = CARTESIAN_POINT ( 'NONE',  ( 17.78000050552179445, -10.16000000000000014, 6.586250505521796583 ) ) ;
#1625 = EDGE_CURVE ( 'NONE', #560, #1840, #3672, .T. ) ;
#1626 = CARTESIAN_POINT ( 'NONE',  ( -8.369992765438043492, 7.901597986548672736, 17.15262445358908039 ) ) ;
#1627 = CARTESIAN_POINT ( 'NONE',  ( -13.86254354666967181, 3.463085079448043668, 32.79636359570053372 ) ) ;
#1628 = LINE ( 'NONE', #462, #4446 ) ;
#1629 = FACE_OUTER_BOUND ( 'NONE', #570, .T. ) ;
#1630 = VERTEX_POINT ( 'NONE', #4058 ) ;
#1631 = FACE_OUTER_BOUND ( 'NONE', #940, .T. ) ;
#1632 = ADVANCED_BREP_SHAPE_REPRESENTATION ( '', ( #1876, #4483 ), #3573 ) ;
#1633 = ORIENTED_EDGE ( 'NONE', *, *, #2504, .F. ) ;
#1634 = PLANE ( 'NONE',  #4302 ) ;
#1635 = CARTESIAN_POINT ( 'NONE',  ( -8.369994990996019624, -6.397499167952784838, 18.40096039353565160 ) ) ;
#1636 = EDGE_LOOP ( 'NONE', ( #2095, #4455, #30, #476, #257 ) ) ;
#1637 = CIRCLE ( 'NONE', #419, 0.5000000000000004441 ) ;
#1638 = DIRECTION ( 'NONE',  ( 0.000000000000000000, 0.000000000000000000, 1.000000000000000000 ) ) ;
#1639 = FACE_OUTER_BOUND ( 'NONE', #1266, .T. ) ;
#1640 = PRODUCT_DEFINITION ( 'UNKNOWN', '', #4328, #1238 ) ;
#1641 = ADVANCED_FACE ( 'NONE', ( #4131 ), #3354, .T. ) ;
#1642 = FACE_OUTER_BOUND ( 'NONE', #2512, .T. ) ;
#1643 = AXIS2_PLACEMENT_3D ( 'NONE', #437, #3683, #394 ) ;
#1644 = VERTEX_POINT ( 'NONE', #910 ) ;
#1645 = ORIENTED_EDGE ( 'NONE', *, *, #3929, .T. ) ;
#1646 = CARTESIAN_POINT ( 'NONE',  ( -14.17127809776796532, 1.877062544604579664, 39.27869980365569091 ) ) ;
#1647 = VECTOR ( 'NONE', #1977, 1000.000000000000000 ) ;
#1648 = DIRECTION ( 'NONE',  ( 0.000000000000000000, 0.000000000000000000, -1.000000000000000000 ) ) ;
#1649 = VERTEX_POINT ( 'NONE', #2309 ) ;
#1650 = CYLINDRICAL_SURFACE ( 'NONE', #1563, 3.573749999999999538 ) ;
#1651 = CARTESIAN_POINT ( 'NONE',  ( -7.619992765438044380, 6.401597986548673624, 31.86762445358908735 ) ) ;
#1652 = CARTESIAN_POINT ( 'NONE',  ( 14.99250723456195189, 0.004097986548670913901, 31.86762445358908735 ) ) ;
#1653 = VECTOR ( 'NONE', #3024, 1000.000000000000000 ) ;
#1654 = CARTESIAN_POINT ( 'NONE',  ( 13.83082084157986458, 3.605824707096489501, 38.55467339862568110 ) ) ;
#1655 = LINE ( 'NONE', #4514, #987 ) ;
#1656 = CARTESIAN_POINT ( 'NONE',  ( 14.20084204937985994, -1.586109036619252288, 35.57693867976828983 ) ) ;
#1657 = VERTEX_POINT ( 'NONE', #2334 ) ;
#1658 = DIRECTION ( 'NONE',  ( 0.000000000000000000, -0.000000000000000000, -1.000000000000000000 ) ) ;
#1659 = ORIENTED_EDGE ( 'NONE', *, *, #1354, .F. ) ;
#1660 = DIRECTION ( 'NONE',  ( 8.673617379884035472E-17, 1.000000000000000000, -0.000000000000000000 ) ) ;
#1661 = AXIS2_PLACEMENT_3D ( 'NONE', #407, #3957, #2829 ) ;
#1662 = ORIENTED_EDGE ( 'NONE', *, *, #4330, .T. ) ;
#1663 = EDGE_CURVE ( 'NONE', #2259, #2212, #4050, .T. ) ;
#1664 = CARTESIAN_POINT ( 'NONE',  ( -3.749999999999999556, 3.750000000000000000, 146.2500000000000000 ) ) ;
#1665 = CIRCLE ( 'NONE', #441, 0.7499999999999997780 ) ;
#1666 = EDGE_CURVE ( 'NONE', #1168, #728, #2646, .T. ) ;
#1667 = LINE ( 'NONE', #1491, #698 ) ;
#1668 = EDGE_LOOP ( 'NONE', ( #3474, #1040, #4467, #3125 ) ) ;
#1669 = ORIENTED_EDGE ( 'NONE', *, *, #3593, .F. ) ;
#1670 = CARTESIAN_POINT ( 'NONE',  ( -14.28749276543804925, 0.004097986548672528061, 17.15262445358908039 ) ) ;
#1671 = ORIENTED_EDGE ( 'NONE', *, *, #3386, .T. ) ;
#1672 = DIRECTION ( 'NONE',  ( 0.000000000000000000, -1.000000000000000000, 0.000000000000000000 ) ) ;
#1673 = AXIS2_PLACEMENT_3D ( 'NONE', #3141, #341, #3480 ) ;
#1674 = CYLINDRICAL_SURFACE ( 'NONE', #1126, 3.573749999999998650 ) ;
#1675 = CARTESIAN_POINT ( 'NONE',  ( -14.09722260588723408, -2.335208591167885039, 39.12537387803049427 ) ) ;
#1676 = CARTESIAN_POINT ( 'NONE',  ( -14.17582932413400698, 1.797604608222738154, 34.96753936920406147 ) ) ;
#1677 = CARTESIAN_POINT ( 'NONE',  ( 3.749999999999999556, -3.750000000000000888, 18.74999999999999645 ) ) ;
#1678 = AXIS2_PLACEMENT_3D ( 'NONE', #2301, #100, #3699 ) ;
#1679 = CARTESIAN_POINT ( 'NONE',  ( -3.573749999999998650, 0.000000000000000000, 1.587499999999999467 ) ) ;
#1680 = PRODUCT_DEFINITION_SHAPE ( 'NONE', 'NONE',  #4650 ) ;
#1681 = DIRECTION ( 'NONE',  ( -1.000000000000000000, -0.000000000000000000, -0.000000000000000000 ) ) ;
#1682 = ORIENTED_EDGE ( 'NONE', *, *, #606, .T. ) ;
#1683 = CARTESIAN_POINT ( 'NONE',  ( 2.316727177394500794E-17, 0.000000000000000000, 11.11249999999999893 ) ) ;
#1684 = CARTESIAN_POINT ( 'NONE',  ( -12.76993906902747611, 6.411095584652301227, 35.55968826673666427 ) ) ;
#1685 = CIRCLE ( 'NONE', #3842, 3.573749999999999538 ) ;
#1686 = ORIENTED_EDGE ( 'NONE', *, *, #2727, .F. ) ;
#1687 = VECTOR ( 'NONE', #2049, 1000.000000000000000 ) ;
#1688 = CARTESIAN_POINT ( 'NONE',  ( 12.37117936981251809, -7.143402013451327193, 32.34872277302695665 ) ) ;
#1689 = DIRECTION ( 'NONE',  ( -1.000000000000000000, 1.076498916035107744E-16, 0.000000000000000000 ) ) ;
#1690 = ORIENTED_EDGE ( 'NONE', *, *, #3764, .T. ) ;
#1691 = ORIENTED_EDGE ( 'NONE', *, *, #527, .T. ) ;
#1692 = LINE ( 'NONE', #1670, #3849 ) ;
#1693 = ORIENTED_EDGE ( 'NONE', *, *, #3936, .T. ) ;
#1694 = FACE_OUTER_BOUND ( 'NONE', #1422, .T. ) ;
#1695 = CIRCLE ( 'NONE', #28, 6.397499999999999964 ) ;
#1696 = CARTESIAN_POINT ( 'NONE',  ( -12.18356754445638934, 7.467360972742721259, 17.28331626890179606 ) ) ;
#1697 = CARTESIAN_POINT ( 'NONE',  ( 12.87888030253338556, -6.192545380470082073, 35.96503381882251205 ) ) ;
#1698 = CARTESIAN_POINT ( 'NONE',  ( 3.750000000000000888, -3.750000000000000000, 146.2500000000000000 ) ) ;
#1699 = EDGE_CURVE ( 'NONE', #3887, #4090, #4106, .T. ) ;
#1700 = EDGE_CURVE ( 'NONE', #4499, #2486, #3753, .T. ) ;
#1701 = CARTESIAN_POINT ( 'NONE',  ( 3.040000505521795571, -17.78000000000000114, 17.28000050552179445 ) ) ;
#1702 = CARTESIAN_POINT ( 'NONE',  ( 14.28750723456195537, 0.004097986548674278397, 17.15262445358908039 ) ) ;
#1703 = DIRECTION ( 'NONE',  ( 0.000000000000000000, 1.000000000000000000, 0.000000000000000000 ) ) ;
#1704 = ORIENTED_EDGE ( 'NONE', *, *, #2927, .T. ) ;
#1705 = CARTESIAN_POINT ( 'NONE',  ( 2.316727177394500794E-17, 0.000000000000000000, 11.11249999999999893 ) ) ;
#1706 = CARTESIAN_POINT ( 'NONE',  ( -8.369992765438045268, -7.143402013451325416, 31.86762445358908735 ) ) ;
#1707 = PRODUCT_DEFINITION_FORMATION_WITH_SPECIFIED_SOURCE ( 'ANY', '', #611, .NOT_KNOWN. ) ;
#1708 = ORIENTED_EDGE ( 'NONE', *, *, #2273, .T. ) ;
#1709 = ORIENTED_EDGE ( 'NONE', *, *, #2190, .F. ) ;
#1710 = AXIS2_PLACEMENT_3D ( 'NONE', #2132, #1813, #2498 ) ;
#1711 = FILL_AREA_STYLE ('',( #590 ) ) ;
#1712 = CIRCLE ( 'NONE', #955, 0.5000000000000004441 ) ;
#1713 = VERTEX_POINT ( 'NONE', #884 ) ;
#1714 = DIRECTION ( 'NONE',  ( -1.000000000000000000, 1.076498916035107621E-16, 0.000000000000000000 ) ) ;
#1715 = EDGE_CURVE ( 'NONE', #3678, #4543, #1665, .T. ) ;
#1716 = CARTESIAN_POINT ( 'NONE',  ( -12.02323085454684026, 7.723227117728908908, 17.16825211198572632 ) ) ;
#1717 = CARTESIAN_POINT ( 'NONE',  ( 12.37117714425454551, -7.147499167952786614, 32.36596039353565857 ) ) ;
#1718 = EDGE_CURVE ( 'NONE', #3472, #1283, #153, .T. ) ;
#1719 = CARTESIAN_POINT ( 'NONE',  ( -9.549434556529077899E-17, -3.249382362871961689E-18, 131.2499999999999716 ) ) ;
#1720 = DIRECTION ( 'NONE',  ( 0.000000000000000000, 0.000000000000000000, 1.000000000000000000 ) ) ;
#1721 = CARTESIAN_POINT ( 'NONE',  ( 17.28000050552179445, -3.039999999999999591, 17.28000050552179445 ) ) ;
#1722 = DIRECTION ( 'NONE',  ( -1.000000000000000000, 1.076498916035107621E-16, 0.000000000000000000 ) ) ;
#1723 = ORIENTED_EDGE ( 'NONE', *, *, #365, .F. ) ;
#1724 = CARTESIAN_POINT ( 'NONE',  ( -13.83332312227014782, 3.573750832047214665, 32.60017139658542362 ) ) ;
#1725 = AXIS2_PLACEMENT_3D ( 'NONE', #4602, #1714, #3137 ) ;
#1726 = ADVANCED_FACE ( 'NONE', ( #1974 ), #1552, .T. ) ;
#1727 = FACE_OUTER_BOUND ( 'NONE', #2682, .T. ) ;
#1728 = ORIENTED_EDGE ( 'NONE', *, *, #996, .T. ) ;
#1729 = VERTEX_POINT ( 'NONE', #3379 ) ;
#1730 = AXIS2_PLACEMENT_3D ( 'NONE', #4300, #413, #763 ) ;
#1731 = SURFACE_SIDE_STYLE ('',( #3135 ) ) ;
#1732 = ADVANCED_FACE ( 'NONE', ( #3429 ), #203, .T. ) ;
#1733 = PRESENTATION_LAYER_ASSIGNMENT (  '', '', ( #1581 ) ) ;
#1734 = EDGE_CURVE ( 'NONE', #2372, #3102, #703, .T. ) ;
#1735 = ORIENTED_EDGE ( 'NONE', *, *, #883, .T. ) ;
#1736 = FACE_OUTER_BOUND ( 'NONE', #1546, .T. ) ;
#1737 = CARTESIAN_POINT ( 'NONE',  ( 8.066546224052645542, -13.73374999999999524, 8.066546224052645542 ) ) ;
#1738 = DIRECTION ( 'NONE',  ( 0.000000000000000000, 0.000000000000000000, 1.000000000000000000 ) ) ;
#1739 = CARTESIAN_POINT ( 'NONE',  ( -14.16478064111921320, -1.882517949369861610, 39.26516300994397568 ) ) ;
#1740 = CARTESIAN_POINT ( 'NONE',  ( 12.51137895040347736, -6.899597777640140706, 34.24694080209222591 ) ) ;
#1741 = CARTESIAN_POINT ( 'NONE',  ( 14.28750500900398279, 8.320472145597748469E-07, 17.65096039353565160 ) ) ;
#1742 = ADVANCED_FACE ( 'NONE', ( #1389, #977 ), #3166, .F. ) ;
#1743 = CIRCLE ( 'NONE', #528, 14.28750000000000142 ) ;
#1744 = DIRECTION ( 'NONE',  ( -1.000000000000000000, 0.000000000000000000, 0.000000000000000000 ) ) ;
#1745 = CARTESIAN_POINT ( 'NONE',  ( -3.749999999999999556, -3.750000000000000888, 131.2499999999999716 ) ) ;
#1746 = CARTESIAN_POINT ( 'NONE',  ( 12.02324532367074639, -7.715031144631558035, 17.16825211198572632 ) ) ;
#1747 = AXIS2_PLACEMENT_3D ( 'NONE', #3292, #107, #2597 ) ;
#1748 = CARTESIAN_POINT ( 'NONE',  ( 17.78000050552179800, -17.78000000000000114, 17.78000050552179445 ) ) ;
#1749 = LINE ( 'NONE', #349, #4366 ) ;
#1750 = AXIS2_PLACEMENT_3D ( 'NONE', #2936, #4047, #3323 ) ;
#1751 = VECTOR ( 'NONE', #4413, 1000.000000000000000 ) ;
#1752 = ORIENTED_EDGE ( 'NONE', *, *, #3349, .T. ) ;
#1753 = EDGE_CURVE ( 'NONE', #3364, #4499, #2698, .T. ) ;
#1754 = CARTESIAN_POINT ( 'NONE',  ( 14.26331614974113116, -0.9480807546542656672, 38.96710911585693538 ) ) ;
#1755 = CARTESIAN_POINT ( 'NONE',  ( -14.28749499099602005, 8.320472117659611842E-07, 35.93971039353566255 ) ) ;
#1756 = ORIENTED_EDGE ( 'NONE', *, *, #3734, .T. ) ;
#1757 = ORIENTED_EDGE ( 'NONE', *, *, #3466, .T. ) ;
#1758 = CARTESIAN_POINT ( 'NONE',  ( -12.37116490068859775, 7.151597986548673624, 31.86762445358908735 ) ) ;
#1759 = ORIENTED_EDGE ( 'NONE', *, *, #647, .F. ) ;
#1760 = CARTESIAN_POINT ( 'NONE',  ( 11.96611785441004372, 7.807463481809645778, 17.65096039353565160 ) ) ;
#1761 = ORIENTED_EDGE ( 'NONE', *, *, #2051, .F. ) ;
#1762 = LINE ( 'NONE', #385, #586 ) ;
#1763 = EDGE_CURVE ( 'NONE', #209, #3059, #3468, .T. ) ;
#1764 = DIRECTION ( 'NONE',  ( -1.076498916035107621E-16, 1.000000000000000000, 0.000000000000000000 ) ) ;
#1765 = CARTESIAN_POINT ( 'NONE',  ( 7.234561953626996335E-06, 0.004097986548672528061, 3.292624453589077405 ) ) ;
#1766 = CARTESIAN_POINT ( 'NONE',  ( 3.040000505521796015, -17.78000000000000114, 3.040000505521795571 ) ) ;
#1767 = VECTOR ( 'NONE', #3192, 1000.000000000000000 ) ;
#1768 = CARTESIAN_POINT ( 'NONE',  ( -8.369992765438045268, -7.143402013451325416, 31.86762445358908735 ) ) ;
#1769 = EDGE_CURVE ( 'NONE', #2126, #3808, #938, .T. ) ;
#1770 = CARTESIAN_POINT ( 'NONE',  ( -14.00292873865404530, 2.840413803447212615, 30.18475356502192142 ) ) ;
#1771 = CARTESIAN_POINT ( 'NONE',  ( -11.96610783640208631, -7.807461817715218189, 17.65096039353565160 ) ) ;
#1772 = CARTESIAN_POINT ( 'NONE',  ( 7.234561953626996335E-06, 0.004097986548672528061, 17.15262445358908039 ) ) ;
#1773 = CARTESIAN_POINT ( 'NONE',  ( 2.316727177394501718E-17, 0.000000000000000000, 4.762500000000001066 ) ) ;
#1774 = ORIENTED_EDGE ( 'NONE', *, *, #4281, .F. ) ;
#1775 = CARTESIAN_POINT ( 'NONE',  ( -8.369994990996016071, 7.897500832047212427, 17.65096039353565160 ) ) ;
#1776 = DIRECTION ( 'NONE',  ( -1.000000000000000000, -0.000000000000000000, -0.000000000000000000 ) ) ;
#1777 = ORIENTED_EDGE ( 'NONE', *, *, #1980, .T. ) ;
#1778 = ORIENTED_EDGE ( 'NONE', *, *, #381, .F. ) ;
#1779 = VERTEX_POINT ( 'NONE', #2781 ) ;
#1780 = CARTESIAN_POINT ( 'NONE',  ( -3.573749999999998650, 0.000000000000000000, 33.33750000000000568 ) ) ;
#1781 = FACE_OUTER_BOUND ( 'NONE', #972, .T. ) ;
#1782 = AXIS2_PLACEMENT_3D ( 'NONE', #1180, #3378, #152 ) ;
#1783 = SHAPE_DEFINITION_REPRESENTATION ( #3171, #2003 ) ;
#1784 = ADVANCED_FACE ( 'NONE', ( #4220 ), #2352, .T. ) ;
#1785 = CARTESIAN_POINT ( 'NONE',  ( 13.05554860573490572, -5.805646240973097783, 36.54145662508980763 ) ) ;
#1786 = AXIS2_PLACEMENT_3D ( 'NONE', #760, #3655, #1532 ) ;
#1787 = LINE ( 'NONE', #1436, #918 ) ;
#1788 = CARTESIAN_POINT ( 'NONE',  ( 17.28000050552179445, -2.539999999999999591, 3.040000505521795571 ) ) ;
#1789 = CARTESIAN_POINT ( 'NONE',  ( 6.870007234561952281, 6.401597986548672736, 17.90262445358908039 ) ) ;
#1790 = CIRCLE ( 'NONE', #1034, 3.573749999999999538 ) ;
#1791 = DIRECTION ( 'NONE',  ( -0.000000000000000000, -0.000000000000000000, -1.000000000000000000 ) ) ;
#1792 = EDGE_CURVE ( 'NONE', #1336, #3535, #1027, .T. ) ;
#1793 = EDGE_CURVE ( 'NONE', #4332, #1428, #3481, .T. ) ;
#1794 = AXIS2_PLACEMENT_3D ( 'NONE', #4458, #879, #1244 ) ;
#1795 = ORIENTED_EDGE ( 'NONE', *, *, #3982, .F. ) ;
#1796 = DIRECTION ( 'NONE',  ( 0.000000000000000000, -1.000000000000000000, 0.000000000000000000 ) ) ;
#1797 = AXIS2_PLACEMENT_3D ( 'NONE', #67, #1085, #1796 ) ;
#1798 = DIRECTION ( 'NONE',  ( 0.000000000000000000, 0.000000000000000000, 1.000000000000000000 ) ) ;
#1799 = EDGE_CURVE ( 'NONE', #2566, #919, #1052, .T. ) ;
#1800 = ORIENTED_EDGE ( 'NONE', *, *, #251, .T. ) ;
#1801 = ORIENTED_EDGE ( 'NONE', *, *, #900, .F. ) ;
#1802 = ADVANCED_FACE ( 'NONE', ( #250 ), #669, .F. ) ;
#1803 =( NAMED_UNIT ( * ) SI_UNIT ( $, .STERADIAN. ) SOLID_ANGLE_UNIT ( ) );
#1804 = ORIENTED_EDGE ( 'NONE', *, *, #2094, .F. ) ;
#1805 = CARTESIAN_POINT ( 'NONE',  ( 12.37117714425454551, 7.147500832047207098, 18.40096039353565160 ) ) ;
#1806 = ORIENTED_EDGE ( 'NONE', *, *, #329, .F. ) ;
#1807 = DIRECTION ( 'NONE',  ( -1.076498916035107621E-16, -1.000000000000000000, 0.000000000000000000 ) ) ;
#1808 = SHAPE_DEFINITION_REPRESENTATION ( #4559, #2171 ) ;
#1809 = CARTESIAN_POINT ( 'NONE',  ( 3.040000505521795571, -17.28000000000000114, 17.78000050552179445 ) ) ;
#1810 = VECTOR ( 'NONE', #130, 1000.000000000000000 ) ;
#1811 = CARTESIAN_POINT ( 'NONE',  ( 14.25915967094480585, -0.9287842060774819108, 28.90698488472980898 ) ) ;
#1812 = DIRECTION ( 'NONE',  ( -1.000000000000000000, 1.076498916035107744E-16, 0.000000000000000000 ) ) ;
#1813 = DIRECTION ( 'NONE',  ( -1.000000000000000000, 0.000000000000000000, 0.000000000000000000 ) ) ;
#1814 = FACE_OUTER_BOUND ( 'NONE', #4308, .T. ) ;
#1815 = CARTESIAN_POINT ( 'NONE',  ( -13.92228970185832360, -3.206939127556818647, 33.45361016550401700 ) ) ;
#1816 = DIRECTION ( 'NONE',  ( 1.000000000000000000, 0.000000000000000000, 0.000000000000000000 ) ) ;
#1817 = ORIENTED_EDGE ( 'NONE', *, *, #1091, .F. ) ;
#1818 = DIRECTION ( 'NONE',  ( 0.000000000000000000, 0.000000000000000000, -1.000000000000000000 ) ) ;
#1819 = PLANE ( 'NONE',  #3250 ) ;
#1820 = PRESENTATION_LAYER_ASSIGNMENT (  '', '', ( #540 ) ) ;
#1821 = CARTESIAN_POINT ( 'NONE',  ( 13.83333536583607959, 3.577847986548670978, 31.86762445358909446 ) ) ;
#1822 = VERTEX_POINT ( 'NONE', #3799 ) ;
#1823 = ORIENTED_EDGE ( 'NONE', *, *, #263, .F. ) ;
#1824 = SHAPE_REPRESENTATION ( 'Part 134_Varsay\X2\0131\X0\lan', ( #4483 ), #3865 ) ;
#1825 = CARTESIAN_POINT ( 'NONE',  ( -12.51136670683754204, 6.903696596236023275, 33.74860486214563338 ) ) ;
#1826 = ORIENTED_EDGE ( 'NONE', *, *, #1666, .T. ) ;
#1827 = DIRECTION ( 'NONE',  ( 0.000000000000000000, 0.000000000000000000, -1.000000000000000000 ) ) ;
#1828 = APPLICATION_PROTOCOL_DEFINITION ( 'draft international standard', 'automotive_design', 1998, #1536 ) ;
#1829 = CARTESIAN_POINT ( 'NONE',  ( 13.66282301451940384, 4.187435799058254027, 37.66764907019537389 ) ) ;
#1830 = DIRECTION ( 'NONE',  ( 1.000000000000000000, 0.000000000000000000, 0.000000000000000000 ) ) ;
#1831 = CARTESIAN_POINT ( 'NONE',  ( 12.37117714425454551, 7.147500832047207098, 18.40096039353565160 ) ) ;
#1832 = AXIS2_PLACEMENT_3D ( 'NONE', #3884, #3837, #3447 ) ;
#1833 = DIRECTION ( 'NONE',  ( 1.000000000000000000, 1.076498916035107621E-16, -0.000000000000000000 ) ) ;
#1834 = EDGE_CURVE ( 'NONE', #3792, #2368, #4246, .T. ) ;
#1835 = DIRECTION ( 'NONE',  ( 0.000000000000000000, 0.000000000000000000, 1.000000000000000000 ) ) ;
#1836 = EDGE_CURVE ( 'NONE', #1947, #3411, #1506, .T. ) ;
#1837 = CARTESIAN_POINT ( 'NONE',  ( -14.20052575156873687, -1.584670739552391128, 35.07725914476921503 ) ) ;
#1838 =( NAMED_UNIT ( * ) PLANE_ANGLE_UNIT ( ) SI_UNIT ( $, .RADIAN. ) );
#1839 = CARTESIAN_POINT ( 'NONE',  ( 14.25916189650278199, -0.9246870515760209353, 28.40864894478323777 ) ) ;
#1840 = VERTEX_POINT ( 'NONE', #3122 ) ;
#1841 = FACE_BOUND ( 'NONE', #3198, .T. ) ;
#1842 = DIRECTION ( 'NONE',  ( 1.000000000000000000, 0.000000000000000000, 0.000000000000000000 ) ) ;
#1843 = ORIENTED_EDGE ( 'NONE', *, *, #2206, .T. ) ;
#1844 = VERTEX_POINT ( 'NONE', #4199 ) ;
#1845 = ORIENTED_EDGE ( 'NONE', *, *, #1590, .F. ) ;
#1846 = VERTEX_POINT ( 'NONE', #3096 ) ;
#1847 = B_SPLINE_CURVE_WITH_KNOTS ( 'NONE', 3,
 ( #4162, #1771, #4251, #1032, #3550, #2452, #1131, #3589, #3613, #2546 ),
 .UNSPECIFIED., .F., .F.,
 ( 4, 2, 2, 2, 4 ),
 ( 0.000000000000000000, 0.0003186827706029867857, 0.0006373655412059735714, 0.0009560483118089603029, 0.001274731082411947143 ),
 .UNSPECIFIED. ) ;
#1848 = CARTESIAN_POINT ( 'NONE',  ( -14.20092307528143216, 1.589399652140962127, 28.65623357306510854 ) ) ;
#1849 = EDGE_CURVE ( 'NONE', #4, #1270, #4277, .T. ) ;
#1850 = CARTESIAN_POINT ( 'NONE',  ( -11.96599547592554025, 7.807632878173365043, 17.65096039353564805 ) ) ;
#1851 = AXIS2_PLACEMENT_3D ( 'NONE', #620, #3796, #4174 ) ;
#1852 = DIRECTION ( 'NONE',  ( -1.000000000000000000, 0.000000000000000000, 0.000000000000000000 ) ) ;
#1853 = CARTESIAN_POINT ( 'NONE',  ( 14.03294480382409937, -2.690185271046441784, 30.00196167051755225 ) ) ;
#1854 = CARTESIAN_POINT ( 'NONE',  ( 7.620007234561951392, 6.401597986548672736, 31.86762445358908735 ) ) ;
#1855 = EDGE_CURVE ( 'NONE', #3011, #1332, #2022, .T. ) ;
#1856 = CARTESIAN_POINT ( 'NONE',  ( 17.78000050552179800, -17.78000000000000114, 17.28000050552179445 ) ) ;
#1857 = DIRECTION ( 'NONE',  ( -0.000000000000000000, -0.000000000000000000, -1.000000000000000000 ) ) ;
#1858 = EDGE_CURVE ( 'NONE', #1623, #2437, #3303, .T. ) ;
#1859 = DIRECTION ( 'NONE',  ( 0.000000000000000000, 0.000000000000000000, 1.000000000000000000 ) ) ;
#1860 = CARTESIAN_POINT ( 'NONE',  ( -13.83332089671217169, -3.569652013451326322, 31.86762445358909446 ) ) ;
#1861 = CARTESIAN_POINT ( 'NONE',  ( 12.18357978802232289, -7.463262154146836913, 17.78165220884836728 ) ) ;
#1862 = VECTOR ( 'NONE', #2981, 1000.000000000000000 ) ;
#1863 = EDGE_LOOP ( 'NONE', ( #3027, #3157, #538, #1526 ) ) ;
#1864 = CARTESIAN_POINT ( 'NONE',  ( -3.749994990996019961, -3.749999167952787094, 3.790960393535649064 ) ) ;
#1865 = VECTOR ( 'NONE', #1286, 1000.000000000000000 ) ;
#1866 = CARTESIAN_POINT ( 'NONE',  ( -13.23941933978631980, -5.369479394468771538, 36.58613208551273033 ) ) ;
#1867 = EDGE_LOOP ( 'NONE', ( #3128, #228, #127, #3376 ) ) ;
#1868 = FACE_OUTER_BOUND ( 'NONE', #2121, .T. ) ;
#1869 = VERTEX_POINT ( 'NONE', #3457 ) ;
#1870 = VERTEX_POINT ( 'NONE', #1698 ) ;
#1871 = DIRECTION ( 'NONE',  ( 9.517981353260378315E-33, 8.841607930564763213E-17, -1.000000000000000000 ) ) ;
#1872 = CARTESIAN_POINT ( 'NONE',  ( 14.24248326661499497, 1.154100376730833544, 28.97554744807429117 ) ) ;
#1873 = CIRCLE ( 'NONE', #813, 3.573750000000000426 ) ;
#1874 = CARTESIAN_POINT ( 'NONE',  ( 0.1449758980921853624, -3.565902013451327068, -9.734783654012170828 ) ) ;
#1875 = EDGE_CURVE ( 'NONE', #3180, #1954, #979, .T. ) ;
#1876 = MANIFOLD_SOLID_BREP ( 'Ölçek1', #1260 ) ;
#1877 = CARTESIAN_POINT ( 'NONE',  ( 12.18303796752544166, 7.468253174740091538, 17.28264009582345651 ) ) ;
#1878 = CARTESIAN_POINT ( 'NONE',  ( 12.37117714425454551, -7.147499167952784838, 17.65096039353565160 ) ) ;
#1879 = AXIS2_PLACEMENT_3D ( 'NONE', #2449, #577, #2423 ) ;
#1880 = CARTESIAN_POINT ( 'NONE',  ( 17.28000050552179800, -17.78000000000000114, 2.540000505521796015 ) ) ;
#1881 = CARTESIAN_POINT ( 'NONE',  ( 14.09186822061629663, -2.358077515305471827, 34.55938405561921201 ) ) ;
#1882 = SURFACE_SIDE_STYLE ('',( #2880 ) ) ;
#1883 = DIRECTION ( 'NONE',  ( 0.000000000000000000, 0.000000000000000000, -1.000000000000000000 ) ) ;
#1884 = ORIENTED_EDGE ( 'NONE', *, *, #1625, .F. ) ;
#1885 = DIRECTION ( 'NONE',  ( -0.000000000000000000, -0.000000000000000000, -1.000000000000000000 ) ) ;
#1886 = CYLINDRICAL_SURFACE ( 'NONE', #3097, 0.7499999999999997780 ) ;
#1887 = ORIENTED_EDGE ( 'NONE', *, *, #4573, .F. ) ;
#1888 = CARTESIAN_POINT ( 'NONE',  ( 8.370005009003978813, -6.397499167952786614, 18.40096039353565160 ) ) ;
#1889 = CARTESIAN_POINT ( 'NONE',  ( 3.040000505521796015, -3.039999999999999147, 3.040000505521795571 ) ) ;
#1890 = PRODUCT_RELATED_PRODUCT_CATEGORY ( 'part', '', ( #4598 ) ) ;
#1891 = AXIS2_PLACEMENT_3D ( 'NONE', #2685, #4123, #2262 ) ;
#1892 = CARTESIAN_POINT ( 'NONE',  ( 10.16000050552179701, -6.586249999999999716, 10.16000050552179701 ) ) ;
#1893 = CIRCLE ( 'NONE', #2479, 0.7500000000000006661 ) ;
#1894 = EDGE_LOOP ( 'NONE', ( #604, #2337, #3690, #2763 ) ) ;
#1895 = B_SPLINE_CURVE_WITH_KNOTS ( 'NONE', 3,
 ( #3963, #736, #4341, #2131, #2571, #2898, #2175, #1770, #2853, #1482, #60, #3567, #1504, #3917, #713, #1130, #672, #3939 ),
 .UNSPECIFIED., .F., .F.,
 ( 4, 2, 2, 2, 2, 2, 2, 2, 4 ),
 ( 0.005610428130223212191, 0.006311357680970753822, 0.007012287231718294586, 0.007713216782465835350, 0.008414146333213377849, 0.009115075883960918612, 0.009816005434708459376, 0.01051693498545600187, 0.01121786453620354437 ),
 .UNSPECIFIED. ) ;
#1896 = ORIENTED_EDGE ( 'NONE', *, *, #4216, .T. ) ;
#1897 = VECTOR ( 'NONE', #690, 1000.000000000000000 ) ;
#1898 = CARTESIAN_POINT ( 'NONE',  ( -13.42336885331644147, 4.896492975942702053, 37.57783078324376191 ) ) ;
#1899 = VERTEX_POINT ( 'NONE', #1002 ) ;
#1900 = SURFACE_SIDE_STYLE ('',( #809 ) ) ;
#1901 = CARTESIAN_POINT ( 'NONE',  ( -3.749999999999999556, 3.750000000000000000, 146.2500000000000000 ) ) ;
#1902 = CARTESIAN_POINT ( 'NONE',  ( 14.28750723456195537, -0.2315532576940860787, 35.44137445358909133 ) ) ;
#1903 = LINE ( 'NONE', #1997, #3009 ) ;
#1904 = CYLINDRICAL_SURFACE ( 'NONE', #3210, 3.573749999999999538 ) ;
#1905 = ADVANCED_FACE ( 'NONE', ( #3142 ), #320, .T. ) ;
#1906 = ORIENTED_EDGE ( 'NONE', *, *, #113, .T. ) ;
#1907 = DIRECTION ( 'NONE',  ( 0.000000000000000000, 1.000000000000000000, 0.000000000000000000 ) ) ;
#1908 = DIRECTION ( 'NONE',  ( 0.000000000000000000, 0.000000000000000000, -1.000000000000000000 ) ) ;
#1909 = DIRECTION ( 'NONE',  ( 0.000000000000000000, -1.000000000000000000, 0.000000000000000000 ) ) ;
#1910 = AXIS2_PLACEMENT_3D ( 'NONE', #632, #3509, #279 ) ;
#1911 = EDGE_LOOP ( 'NONE', ( #1265, #4334, #383, #1669 ) ) ;
#1912 = CARTESIAN_POINT ( 'NONE',  ( 13.83333536583607604, -3.569652013451329875, 31.63041714010483219 ) ) ;
#1913 = CARTESIAN_POINT ( 'NONE',  ( 12.37117936981251987, 7.151597986548670072, 31.86762445358908735 ) ) ;
#1914 = LINE ( 'NONE', #2256, #2932 ) ;
#1915 = DIRECTION ( 'NONE',  ( -1.000000000000000000, -1.076498916035107621E-16, 0.000000000000000000 ) ) ;
#1916 = ORIENTED_EDGE ( 'NONE', *, *, #1663, .F. ) ;
#1917 = ORIENTED_EDGE ( 'NONE', *, *, #2467, .F. ) ;
#1918 = ITEM_DEFINED_TRANSFORMATION ( 'NONE', 'NONE', #2361,  #4483 ) ;
#1919 = CARTESIAN_POINT ( 'NONE',  ( -12.13219254000220459, -7.542609400219328464, 17.23334239392281475 ) ) ;
#1920 = MANIFOLD_SOLID_BREP ( 'Ölçek1', #3278 ) ;
#1921 = ORIENTED_EDGE ( 'NONE', *, *, #894, .F. ) ;
#1922 = FILL_AREA_STYLE ('',( #2968 ) ) ;
#1923 = EDGE_CURVE ( 'NONE', #4497, #1497, #2326, .T. ) ;
#1924 = DIRECTION ( 'NONE',  ( -8.673617379884035472E-17, -1.000000000000000000, 0.000000000000000000 ) ) ;
#1925 = CARTESIAN_POINT ( 'NONE',  ( -13.94750378805149360, 3.105294744008160635, 33.65912111070095136 ) ) ;
#1926 = FACE_OUTER_BOUND ( 'NONE', #2444, .T. ) ;
#1927 = CARTESIAN_POINT ( 'NONE',  ( -7.619994990996019624, 8.320472136303528048E-07, 32.36596039353565857 ) ) ;
#1928 =( BOUNDED_CURVE ( )  B_SPLINE_CURVE ( 3, ( #4252, #4586, #4182, #1033 ),
 .UNSPECIFIED., .F., .F. ) 
 B_SPLINE_CURVE_WITH_KNOTS ( ( 4, 4 ),
 ( 1.570796326794896558, 3.141592653589793116 ),
 .UNSPECIFIED. ) 
 CURVE ( )  GEOMETRIC_REPRESENTATION_ITEM ( )  RATIONAL_B_SPLINE_CURVE ( ( 1.000000000000000000, 0.8047378541243649375, 0.8047378541243649375, 1.000000000000000000 ) ) 
 REPRESENTATION_ITEM ( '' )  );
#1929 = ORIENTED_EDGE ( 'NONE', *, *, #3279, .T. ) ;
#1930 = DIRECTION ( 'NONE',  ( 0.000000000000000000, 0.000000000000000000, 1.000000000000000000 ) ) ;
#1931 = AXIS2_PLACEMENT_3D ( 'NONE', #1371, #3172, #673 ) ;
#1932 = CARTESIAN_POINT ( 'NONE',  ( 7.620007234561951392, 6.401597986548672736, 17.90262445358908039 ) ) ;
#1933 = EDGE_CURVE ( 'NONE', #657, #3907, #4374, .T. ) ;
#1934 = EDGE_CURVE ( 'NONE', #724, #4479, #108, .T. ) ;
#1935 = CARTESIAN_POINT ( 'NONE',  ( -4.762492765438045339, 0.004097986548673111795, -10.04237554641092345 ) ) ;
#1936 = ORIENTED_EDGE ( 'NONE', *, *, #4404, .F. ) ;
#1937 = CARTESIAN_POINT ( 'NONE',  ( -6.869992765438044380, 12.08996809382683857, 17.90262445358908039 ) ) ;
#1938 = ADVANCED_FACE ( 'NONE', ( #1926 ), #2336, .F. ) ;
#1939 = CARTESIAN_POINT ( 'NONE',  ( 17.28000050552179800, -17.28000000000000114, 3.040000505521795571 ) ) ;
#1940 = CIRCLE ( 'NONE', #207, 14.28750000000000142 ) ;
#1941 = ORIENTED_EDGE ( 'NONE', *, *, #163, .T. ) ;
#1942 = VERTEX_POINT ( 'NONE', #1604 ) ;
#1943 = ITEM_DEFINED_TRANSFORMATION ( 'NONE', 'NONE', #3041,  #4483 ) ;
#1944 = CARTESIAN_POINT ( 'NONE',  ( -9.549434556529077899E-17, -3.249382362871961689E-18, 131.2499999999999716 ) ) ;
#1945 = CARTESIAN_POINT ( 'NONE',  ( -12.37116490068861552, -7.143402013451322752, 17.79394892777614601 ) ) ;
#1946 = VECTOR ( 'NONE', #325, 1000.000000000000000 ) ;
#1947 = VERTEX_POINT ( 'NONE', #3019 ) ;
#1948 = DIRECTION ( 'NONE',  ( -0.000000000000000000, -0.000000000000000000, -1.000000000000000000 ) ) ;
#1949 = CARTESIAN_POINT ( 'NONE',  ( 3.573749999999998650, 4.376581498452851814E-16, 33.33750000000000568 ) ) ;
#1950 = DIRECTION ( 'NONE',  ( 1.000000000000000000, 0.000000000000000000, 0.000000000000000000 ) ) ;
#1951 = CARTESIAN_POINT ( 'NONE',  ( 12.87896032641104505, 6.192408470356285832, 35.96538579746960806 ) ) ;
#1952 = CARTESIAN_POINT ( 'NONE',  ( -8.369992765438043492, 6.401597986548673624, 3.292624453589077405 ) ) ;
#1953 = DIRECTION ( 'NONE',  ( 1.000000000000000000, 0.000000000000000000, 0.000000000000000000 ) ) ;
#1954 = VERTEX_POINT ( 'NONE', #4133 ) ;
#1955 = FACE_OUTER_BOUND ( 'NONE', #2612, .T. ) ;
#1956 = CARTESIAN_POINT ( 'NONE',  ( 14.28155886016486598, 0.4760400057381644068, 28.31745088146499967 ) ) ;
#1957 = COLOUR_RGB ( '', 0.40784314, 0.44705882, 0.49803922) ;
#1958 = CARTESIAN_POINT ( 'NONE',  ( 14.99250500900397753, 8.320472111961197689E-07, 32.36596039353565857 ) ) ;
#1959 = ORIENTED_EDGE ( 'NONE', *, *, #1793, .T. ) ;
#1960 = CARTESIAN_POINT ( 'NONE',  ( -17.48249499099600968, -7.147499167952782173, 3.790960393535648176 ) ) ;
#1961 = CARTESIAN_POINT ( 'NONE',  ( -13.94750601360946796, 3.101197589506698993, 34.15745705064754389 ) ) ;
#1962 = ADVANCED_FACE ( 'NONE', ( #1577 ), #1976, .T. ) ;
#1963 = CARTESIAN_POINT ( 'NONE',  ( 17.78000050552179445, -3.039999999999999591, 17.78000050552179445 ) ) ;
#1964 = AXIS2_PLACEMENT_3D ( 'NONE', #1748, #3173, #4611 ) ;
#1965 = CARTESIAN_POINT ( 'NONE',  ( -7.619994990996017847, 6.397500832047212427, 18.40096039353565160 ) ) ;
#1966 = EDGE_CURVE ( 'NONE', #4397, #975, #307, .T. ) ;
#1967 = ORIENTED_EDGE ( 'NONE', *, *, #3940, .F. ) ;
#1968 = VECTOR ( 'NONE', #2812, 1000.000000000000000 ) ;
#1969 = ORIENTED_EDGE ( 'NONE', *, *, #2066, .F. ) ;
#1970 = DIRECTION ( 'NONE',  ( -0.000000000000000000, -1.000000000000000000, -0.000000000000000000 ) ) ;
#1971 = VECTOR ( 'NONE', #2221, 1000.000000000000000 ) ;
#1972 = EDGE_LOOP ( 'NONE', ( #2357, #1671 ) ) ;
#1973 = DIRECTION ( 'NONE',  ( -1.000000000000000000, 0.000000000000000000, -0.000000000000000000 ) ) ;
#1974 = FACE_OUTER_BOUND ( 'NONE', #3051, .T. ) ;
#1975 = CARTESIAN_POINT ( 'NONE',  ( -9.549434556529077899E-17, 3.750000000000000000, 146.2500000000000000 ) ) ;
#1976 = CYLINDRICAL_SURFACE ( 'NONE', #3838, 3.573749999999999538 ) ;
#1977 = DIRECTION ( 'NONE',  ( 1.000000000000000000, -0.000000000000000000, -0.000000000000000000 ) ) ;
#1978 = ORIENTED_EDGE ( 'NONE', *, *, #3883, .T. ) ;
#1979 = CARTESIAN_POINT ( 'NONE',  ( 12.35746789565908799, -7.167253453071094960, 17.68815867240257589 ) ) ;
#1980 = EDGE_CURVE ( 'NONE', #567, #675, #2290, .T. ) ;
#1981 = ORIENTED_EDGE ( 'NONE', *, *, #647, .T. ) ;
#1982 = LINE ( 'NONE', #2027, #839 ) ;
#1983 = ORIENTED_EDGE ( 'NONE', *, *, #4335, .F. ) ;
#1984 = CARTESIAN_POINT ( 'NONE',  ( -8.369994990996019624, -6.397499167952783061, 3.790960393535648176 ) ) ;
#1985 = FACE_OUTER_BOUND ( 'NONE', #837, .T. ) ;
#1986 = CYLINDRICAL_SURFACE ( 'NONE', #722, 3.573750000000000426 ) ;
#1987 = ORIENTED_EDGE ( 'NONE', *, *, #429, .T. ) ;
#1988 = CARTESIAN_POINT ( 'NONE',  ( 17.78000050552179445, -2.539999999999999591, 17.28000050552179445 ) ) ;
#1989 = CARTESIAN_POINT ( 'NONE',  ( 5.009003980371977336E-06, 3.750000832047212906, 17.65096039353565160 ) ) ;
#1990 = UNCERTAINTY_MEASURE_WITH_UNIT (LENGTH_MEASURE( 1.000000000000000082E-05 ), #3935, 'distance_accuracy_value', 'NONE');
#1991 = ORIENTED_EDGE ( 'NONE', *, *, #3877, .T. ) ;
#1992 = EDGE_CURVE ( 'NONE', #3326, #3048, #2311, .T. ) ;
#1993 = PLANE ( 'NONE',  #2010 ) ;
#1994 = PRODUCT_DEFINITION_SHAPE ( 'NONE', 'NONE',  #4660 ) ;
#1995 = CARTESIAN_POINT ( 'NONE',  ( 8.370005009003980589, -7.147499167952786614, 32.36596039353565857 ) ) ;
#1996 = DIRECTION ( 'NONE',  ( -1.000000000000000000, 0.000000000000000000, 0.000000000000000000 ) ) ;
#1997 = CARTESIAN_POINT ( 'NONE',  ( 8.370007234561949616, 7.151597986548671848, 31.86762445358908735 ) ) ;
#1998 = ADVANCED_FACE ( 'NONE', ( #886 ), #483, .T. ) ;
#1999 = CARTESIAN_POINT ( 'NONE',  ( 13.86272383238697969, -3.458313573812046737, 33.29701817273350173 ) ) ;
#2000 = ORIENTED_EDGE ( 'NONE', *, *, #4375, .T. ) ;
#2001 = EDGE_CURVE ( 'NONE', #992, #975, #508, .T. ) ;
#2002 = CARTESIAN_POINT ( 'NONE',  ( 12.18358201358030080, -7.459164999645373939, 17.28331626890179606 ) ) ;
#2003 = SHAPE_REPRESENTATION ( 'Part 133_Varsay\X2\0131\X0\lan', ( #4483 ), #2816 ) ;
#2004 = ORIENTED_EDGE ( 'NONE', *, *, #406, .F. ) ;
#2005 = CARTESIAN_POINT ( 'NONE',  ( -17.48249276543803532, -7.143402013451320975, 3.292624453589076960 ) ) ;
#2006 = VERTEX_POINT ( 'NONE', #182 ) ;
#2007 = CIRCLE ( 'NONE', #3202, 4.762499999999999289 ) ;
#2008 = DIRECTION ( 'NONE',  ( 1.000000000000000000, -0.000000000000000000, -0.000000000000000000 ) ) ;
#2009 = DIRECTION ( 'NONE',  ( -1.000000000000000000, 0.000000000000000000, 0.000000000000000000 ) ) ;
#2010 = AXIS2_PLACEMENT_3D ( 'NONE', #3426, #4128, #2061 ) ;
#2011 = EDGE_LOOP ( 'NONE', ( #1090, #449, #4613, #589 ) ) ;
#2012 = B_SPLINE_CURVE_WITH_KNOTS ( 'NONE', 3,
 ( #576, #3355, #3754, #1226, #3430, #2647, #1676, #556, #181, #912, #1204, #1925, #1576, #933, #1627, #131, #3018, #4059 ),
 .UNSPECIFIED., .F., .F.,
 ( 4, 2, 2, 2, 2, 2, 2, 2, 4 ),
 ( 1.014745470810651806E-18, 0.0007013035162779033670, 0.001402607032555805867, 0.002103910548833708150, 0.002805214065111610432, 0.003506517581389512715, 0.004207821097667415432, 0.004909124613945317281, 0.005610428130223219997 ),
 .UNSPECIFIED. ) ;
#2013 = APPLICATION_CONTEXT ( 'automotive_design' ) ;
#2014 = VERTEX_POINT ( 'NONE', #3707 ) ;
#2015 = CIRCLE ( 'NONE', #4642, 0.7500000000000006661 ) ;
#2016 = ORIENTED_EDGE ( 'NONE', *, *, #3793, .F. ) ;
#2017 = DIRECTION ( 'NONE',  ( -0.000000000000000000, -0.000000000000000000, -1.000000000000000000 ) ) ;
#2018 =( NAMED_UNIT ( * ) PLANE_ANGLE_UNIT ( ) SI_UNIT ( $, .RADIAN. ) );
#2019 = CARTESIAN_POINT ( 'NONE',  ( -14.19372585200764014, -1.650818847648656940, 39.32424842390233977 ) ) ;
#2020 = AXIS2_PLACEMENT_3D ( 'NONE', #1306, #2251, #1658 ) ;
#2021 = CARTESIAN_POINT ( 'NONE',  ( 14.28750500900398102, 0.4809648669972392265, 39.51346039353565232 ) ) ;
#2022 = LINE ( 'NONE', #2807, #4353 ) ;
#2023 = FACE_OUTER_BOUND ( 'NONE', #2011, .T. ) ;
#2024 = ORIENTED_EDGE ( 'NONE', *, *, #4082, .T. ) ;
#2025 = DIRECTION ( 'NONE',  ( 0.000000000000000000, 0.000000000000000000, -1.000000000000000000 ) ) ;
#2026 = VERTEX_POINT ( 'NONE', #3044 ) ;
#2027 = CARTESIAN_POINT ( 'NONE',  ( 5.009003980046716684E-06, -3.749999167952787538, 17.65096039353565160 ) ) ;
#2028 = VECTOR ( 'NONE', #3476, 1000.000000000000000 ) ;
#2029 = ORIENTED_EDGE ( 'NONE', *, *, #1753, .T. ) ;
#2030 = CARTESIAN_POINT ( 'NONE',  ( -14.28749499099602005, 8.320472117659611842E-07, 35.93971039353566255 ) ) ;
#2031 = VECTOR ( 'NONE', #3042, 1000.000000000000000 ) ;
#2032 = PRODUCT_DEFINITION_SHAPE ( 'NONE', 'NONE',  #4657 ) ;
#2033 = ORIENTED_EDGE ( 'NONE', *, *, #3116, .T. ) ;
#2034 = ORIENTED_EDGE ( 'NONE', *, *, #748, .F. ) ;
#2035 = ADVANCED_FACE ( 'NONE', ( #1227 ), #1275, .T. ) ;
#2036 = DIRECTION ( 'NONE',  ( -0.000000000000000000, -0.000000000000000000, -1.000000000000000000 ) ) ;
#2037 = ORIENTED_EDGE ( 'NONE', *, *, #2094, .T. ) ;
#2038 = DIRECTION ( 'NONE',  ( 1.000000000000000000, 0.000000000000000000, 0.000000000000000000 ) ) ;
#2039 = TOROIDAL_SURFACE ( 'NONE', #4285, 1.500000000000000000, 0.7500000000000000000 ) ;
#2040 = CARTESIAN_POINT ( 'NONE',  ( 8.370005009003978813, -6.397499167952786614, 18.40096039353565160 ) ) ;
#2041 = EDGE_CURVE ( 'NONE', #3102, #1623, #1628, .T. ) ;
#2042 = DIRECTION ( 'NONE',  ( 0.000000000000000000, 0.000000000000000000, 1.000000000000000000 ) ) ;
#2043 = CARTESIAN_POINT ( 'NONE',  ( 13.30084886853356707, -5.220167152536361321, 37.25360547957400570 ) ) ;
#2044 = CARTESIAN_POINT ( 'NONE',  ( 8.370005009003978813, 7.897500832047212427, 18.40096039353565160 ) ) ;
#2045 = CARTESIAN_POINT ( 'NONE',  ( -14.28749276543804925, 0.004097986548672528061, 28.29387445358909403 ) ) ;
#2046 = PRODUCT_DEFINITION_SHAPE ( 'NONE', 'NONE',  #4653 ) ;
#2047 = CARTESIAN_POINT ( 'NONE',  ( 2.540000505521796015, -17.78000000000000114, 3.040000505521795571 ) ) ;
#2048 = ORIENTED_EDGE ( 'NONE', *, *, #2959, .T. ) ;
#2049 = DIRECTION ( 'NONE',  ( 1.000000000000000000, 8.673617379884035472E-17, -0.000000000000000000 ) ) ;
#2050 = AXIS2_PLACEMENT_3D ( 'NONE', #2608, #4046, #844 ) ;
#2051 = EDGE_CURVE ( 'NONE', #2260, #1488, #3779, .T. ) ;
#2052 = VERTEX_POINT ( 'NONE', #557 ) ;
#2053 = AXIS2_PLACEMENT_3D ( 'NONE', #2005, #3001, #4422 ) ;
#2054 = DIRECTION ( 'NONE',  ( 1.000000000000000000, 0.000000000000000000, 0.000000000000000000 ) ) ;
#2055 = LINE ( 'NONE', #2366, #3134 ) ;
#2056 = ORIENTED_EDGE ( 'NONE', *, *, #3152, .F. ) ;
#2057 = VECTOR ( 'NONE', #4529, 1000.000000000000000 ) ;
#2058 = ORIENTED_EDGE ( 'NONE', *, *, #62, .F. ) ;
#2059 =( NAMED_UNIT ( * ) PLANE_ANGLE_UNIT ( ) SI_UNIT ( $, .RADIAN. ) );
#2060 = ORIENTED_EDGE ( 'NONE', *, *, #3279, .F. ) ;
#2061 = DIRECTION ( 'NONE',  ( -1.000000000000000000, 0.000000000000000000, -0.000000000000000000 ) ) ;
#2062 = CIRCLE ( 'NONE', #2799, 0.5000000000000000000 ) ;
#2063 = FACE_OUTER_BOUND ( 'NONE', #26, .T. ) ;
#2064 = CARTESIAN_POINT ( 'NONE',  ( -13.42355275005542303, -4.895986476802388410, 37.57830303755702062 ) ) ;
#2065 = DIRECTION ( 'NONE',  ( 0.000000000000000000, 0.000000000000000000, 1.000000000000000000 ) ) ;
#2066 = EDGE_CURVE ( 'NONE', #4, #2259, #1903, .T. ) ;
#2067 = CARTESIAN_POINT ( 'NONE',  ( 14.03294512273307859, -2.690168477928161828, 34.72994684450105751 ) ) ;
#2068 = ADVANCED_BREP_SHAPE_REPRESENTATION ( '', ( #391, #4483 ), #2816 ) ;
#2069 = LINE ( 'NONE', #2047, #3800 ) ;
#2070 = CARTESIAN_POINT ( 'NONE',  ( 7.620007234561953169, 3.577847986548671422, 31.86762445358909446 ) ) ;
#2071 = CARTESIAN_POINT ( 'NONE',  ( 3.750005009003979595, -3.749999167952787538, 3.790960393535649064 ) ) ;
#2072 =( REPRESENTATION_RELATIONSHIP ('NONE','NONE', #4401, #2171 ) REPRESENTATION_RELATIONSHIP_WITH_TRANSFORMATION ( #147 )SHAPE_REPRESENTATION_RELATIONSHIP( ) );
#2073 = ORIENTED_EDGE ( 'NONE', *, *, #3677, .F. ) ;
#2074 = CARTESIAN_POINT ( 'NONE',  ( 12.76995131259341498, -6.406996766056419546, 35.06135232679011438 ) ) ;
#2075 = EDGE_CURVE ( 'NONE', #1899, #1408, #1301, .T. ) ;
#2076 = EDGE_CURVE ( 'NONE', #1729, #4385, #1655, .T. ) ;
#2077 = DIRECTION ( 'NONE',  ( 0.000000000000000000, 0.000000000000000000, 1.000000000000000000 ) ) ;
#2078 = ORIENTED_EDGE ( 'NONE', *, *, #865, .T. ) ;
#2079 = EDGE_LOOP ( 'NONE', ( #2567, #3014, #4031, #2442 ) ) ;
#2080 = EDGE_CURVE ( 'NONE', #3952, #1143, #1047, .T. ) ;
#2081 = CARTESIAN_POINT ( 'NONE',  ( 13.73375050552179744, -10.16000000000000014, 6.586250505521794807 ) ) ;
#2082 = ORIENTED_EDGE ( 'NONE', *, *, #3999, .F. ) ;
#2083 = DIRECTION ( 'NONE',  ( 0.000000000000000000, 0.000000000000000000, 1.000000000000000000 ) ) ;
#2084 = CARTESIAN_POINT ( 'NONE',  ( 17.28000050552179800, -17.78000000000000114, 3.040000505521795571 ) ) ;
#2085 = DIRECTION ( 'NONE',  ( 1.000000000000000000, 0.000000000000000000, 0.000000000000000000 ) ) ;
#2086 = CARTESIAN_POINT ( 'NONE',  ( 2.540000505521795127, -17.28000000000000114, 2.540000505521796015 ) ) ;
#2087 = DIRECTION ( 'NONE',  ( -0.000000000000000000, -0.000000000000000000, 1.000000000000000000 ) ) ;
#2088 = DIRECTION ( 'NONE',  ( -0.000000000000000000, -0.000000000000000000, 1.000000000000000000 ) ) ;
#2089 = DIRECTION ( 'NONE',  ( 0.000000000000000000, 0.000000000000000000, -1.000000000000000000 ) ) ;
#2090 = DIRECTION ( 'NONE',  ( -1.000000000000000000, 0.000000000000000000, 0.000000000000000000 ) ) ;
#2091 = VERTEX_POINT ( 'NONE', #2871 ) ;
#2092 = DIRECTION ( 'NONE',  ( 1.000000000000000000, 0.000000000000000000, 0.000000000000000000 ) ) ;
#2093 = CARTESIAN_POINT ( 'NONE',  ( 6.586250505521797471, -10.16000000000000014, 17.78000050552179445 ) ) ;
#2094 = EDGE_CURVE ( 'NONE', #2828, #2091, #2516, .T. ) ;
#2095 = ORIENTED_EDGE ( 'NONE', *, *, #667, .F. ) ;
#2096 = TOROIDAL_SURFACE ( 'NONE', #3461, 1.500000000000000000, 0.7500000000000000000 ) ;
#2097 = CARTESIAN_POINT ( 'NONE',  ( -14.28749276543804569, 0.004097986548671483757, 35.44137445358909133 ) ) ;
#2098 = EDGE_CURVE ( 'NONE', #3403, #3411, #1097, .T. ) ;
#2099 = ORIENTED_EDGE ( 'NONE', *, *, #3256, .T. ) ;
#2100 = DIRECTION ( 'NONE',  ( 0.000000000000000000, 1.000000000000000000, 0.000000000000000000 ) ) ;
#2101 = ORIENTED_EDGE ( 'NONE', *, *, #4428, .F. ) ;
#2102 = DIRECTION ( 'NONE',  ( -1.000000000000000000, 0.000000000000000000, 8.673617379884026597E-16 ) ) ;
#2103 = DIRECTION ( 'NONE',  ( 8.711406316995871891E-17, 0.8092350291518397576, 0.5874850360593205645 ) ) ;
#2104 = CARTESIAN_POINT ( 'NONE',  ( -13.30104869160269665, -5.219631826751473191, 37.25417504454090789 ) ) ;
#2105 = CYLINDRICAL_SURFACE ( 'NONE', #1673, 0.7499999999999997780 ) ;
#2106 = TOROIDAL_SURFACE ( 'NONE', #2179, 1.500000000000000000, 0.7500000000000000000 ) ;
#2107 = CIRCLE ( 'NONE', #2253, 3.573749999999999538 ) ;
#2108 = CYLINDRICAL_SURFACE ( 'NONE', #2115, 14.28750000000000142 ) ;
#2109 = LINE ( 'NONE', #3124, #726 ) ;
#2110 = AXIS2_PLACEMENT_3D ( 'NONE', #2289, #861, #834 ) ;
#2111 = CARTESIAN_POINT ( 'NONE',  ( 14.28750500900398279, 8.320472145597748469E-07, 39.51346039353565942 ) ) ;
#2112 = DIRECTION ( 'NONE',  ( -1.000000000000000000, -0.000000000000000000, -0.000000000000000000 ) ) ;
#2113 = PRESENTATION_LAYER_ASSIGNMENT (  '', '', ( #4292 ) ) ;
#2114 = VECTOR ( 'NONE', #695, 1000.000000000000000 ) ;
#2115 = AXIS2_PLACEMENT_3D ( 'NONE', #2920, #1157, #2149 ) ;
#2116 = ORIENTED_EDGE ( 'NONE', *, *, #2744, .T. ) ;
#2117 = DIRECTION ( 'NONE',  ( 1.000000000000000000, -1.076498916035107621E-16, -0.000000000000000000 ) ) ;
#2118 = PRODUCT_DEFINITION_SHAPE ( 'NONE', 'NONE',  #500 ) ;
#2119 = CARTESIAN_POINT ( 'NONE',  ( -3.573749999999998650, 0.000000000000000000, 4.762500000000001066 ) ) ;
#2120 = EDGE_LOOP ( 'NONE', ( #1723, #2169 ) ) ;
#2121 = EDGE_LOOP ( 'NONE', ( #1262, #140, #755, #1475 ) ) ;
#2122 = EDGE_CURVE ( 'NONE', #3671, #2770, #3956, .T. ) ;
#2123 = FILL_AREA_STYLE ('',( #1405 ) ) ;
#2124 = ORIENTED_EDGE ( 'NONE', *, *, #1247, .F. ) ;
#2125 = LINE ( 'NONE', #1780, #3439 ) ;
#2126 = VERTEX_POINT ( 'NONE', #2708 ) ;
#2127 = CARTESIAN_POINT ( 'NONE',  ( 11.90639614989970063, -7.897499167952783949, 17.65096039353565160 ) ) ;
#2128 = EDGE_CURVE ( 'NONE', #2747, #3571, #1267, .T. ) ;
#2129 = CARTESIAN_POINT ( 'NONE',  ( 13.66253082644668027, -4.184297042924940868, 38.16530575332426167 ) ) ;
#2130 = AXIS2_PLACEMENT_3D ( 'NONE', #1426, #1776, #2505 ) ;
#2131 = CARTESIAN_POINT ( 'NONE',  ( -13.86271395683116836, 3.458313116067174953, 31.43508225166169368 ) ) ;
#2132 = CARTESIAN_POINT ( 'NONE',  ( 17.78000050552179445, -10.16000000000000014, 10.16000050552179701 ) ) ;
#2133 = DIRECTION ( 'NONE',  ( 0.000000000000000000, 0.000000000000000000, 1.000000000000000000 ) ) ;
#2134 = PLANE ( 'NONE',  #911 ) ;
#2135 = EDGE_CURVE ( 'NONE', #4121, #1846, #1599, .T. ) ;
#2136 = ADVANCED_FACE ( 'NONE', ( #1243 ), #3747, .T. ) ;
#2137 = ORIENTED_EDGE ( 'NONE', *, *, #2900, .F. ) ;
#2138 = CARTESIAN_POINT ( 'NONE',  ( 3.040000505521796015, -3.039999999999999591, 17.78000050552179445 ) ) ;
#2139 = PLANE ( 'NONE',  #3558 ) ;
#2140 = ORIENTED_EDGE ( 'NONE', *, *, #1663, .T. ) ;
#2141 = ORIENTED_EDGE ( 'NONE', *, *, #1992, .T. ) ;
#2142 = CARTESIAN_POINT ( 'NONE',  ( 10.16000050552179701, -10.16000000000000014, 2.540000505521796015 ) ) ;
#2143 = ORIENTED_EDGE ( 'NONE', *, *, #114, .T. ) ;
#2144 = FACE_OUTER_BOUND ( 'NONE', #4550, .T. ) ;
#2145 = LINE ( 'NONE', #3582, #2908 ) ;
#2146 = CIRCLE ( 'NONE', #2967, 0.7499999999999997780 ) ;
#2147 = PRODUCT_CONTEXT ( 'NONE', #3119, 'mechanical' ) ;
#2148 = CARTESIAN_POINT ( 'NONE',  ( 13.60392424361874575, 4.374602804431722447, 37.52789170789245787 ) ) ;
#2149 = DIRECTION ( 'NONE',  ( -1.000000000000000000, 0.000000000000000000, 0.000000000000000000 ) ) ;
#2150 =( REPRESENTATION_RELATIONSHIP ('NONE','NONE', #4401, #2171 ) REPRESENTATION_RELATIONSHIP_WITH_TRANSFORMATION ( #4480 )SHAPE_REPRESENTATION_RELATIONSHIP( ) );
#2151 = EDGE_CURVE ( 'NONE', #1840, #4649, #2663, .T. ) ;
#2152 = CARTESIAN_POINT ( 'NONE',  ( 8.370005009003978813, 7.147500832047211539, 32.36596039353565857 ) ) ;
#2153 = DIRECTION ( 'NONE',  ( -1.000000000000000000, 0.000000000000000000, 0.000000000000000000 ) ) ;
#2154 = FACE_OUTER_BOUND ( 'NONE', #2481, .T. ) ;
#2155 = AXIS2_PLACEMENT_3D ( 'NONE', #1135, #765, #3293 ) ;
#2156 = FACE_OUTER_BOUND ( 'NONE', #4381, .T. ) ;
#2157 = FACE_BOUND ( 'NONE', #4313, .T. ) ;
#2158 = ORIENTED_EDGE ( 'NONE', *, *, #2269, .F. ) ;
#2159 = CARTESIAN_POINT ( 'NONE',  ( 14.28750500900398634, 0.2357416791107340981, 35.93971039353567676 ) ) ;
#2160 = CARTESIAN_POINT ( 'NONE',  ( 18.74250500900397753, 8.320472107924325483E-07, 32.36596039353566567 ) ) ;
#2161 = AXIS2_PLACEMENT_3D ( 'NONE', #210, #3000, #1232 ) ;
#2162 = CARTESIAN_POINT ( 'NONE',  ( 3.750000000000000888, -3.750000000000000000, 146.2500000000000000 ) ) ;
#2163 = AXIS2_PLACEMENT_3D ( 'NONE', #3029, #3788, #2703 ) ;
#2164 = ORIENTED_EDGE ( 'NONE', *, *, #1393, .T. ) ;
#2165 = ORIENTED_EDGE ( 'NONE', *, *, #3906, .F. ) ;
#2166 = CARTESIAN_POINT ( 'NONE',  ( -13.48424197071718567, 4.730921210558564738, 37.23391125615017927 ) ) ;
#2167 = ORIENTED_EDGE ( 'NONE', *, *, #280, .T. ) ;
#2168 = ADVANCED_FACE ( 'NONE', ( #4101 ), #1290, .F. ) ;
#2169 = ORIENTED_EDGE ( 'NONE', *, *, #923, .F. ) ;
#2170 = FACE_OUTER_BOUND ( 'NONE', #926, .T. ) ;
#2171 = SHAPE_REPRESENTATION ( 'Part 135_Varsay\X2\0131\X0\lan', ( #4483 ), #3573 ) ;
#2172 = CIRCLE ( 'NONE', #4357, 0.5000000000000004441 ) ;
#2173 = CARTESIAN_POINT ( 'NONE',  ( 13.11703699520739441, 5.669897148686642296, 36.23092228855527708 ) ) ;
#2174 = EDGE_CURVE ( 'NONE', #2259, #2006, #236, .T. ) ;
#2175 = CARTESIAN_POINT ( 'NONE',  ( -13.94802723912598097, 3.098790239948968850, 30.57065727641915132 ) ) ;
#2176 = DIRECTION ( 'NONE',  ( -1.000000000000000000, 0.000000000000000000, 0.000000000000000000 ) ) ;
#2177 = DIRECTION ( 'NONE',  ( -1.000000000000000000, 0.000000000000000000, 0.000000000000000000 ) ) ;
#2178 = CARTESIAN_POINT ( 'NONE',  ( -7.619992765438044380, 12.08996809382683857, 39.01512445358908110 ) ) ;
#2179 = AXIS2_PLACEMENT_3D ( 'NONE', #3942, #1133, #3308 ) ;
#2180 = CARTESIAN_POINT ( 'NONE',  ( -13.94746062085793881, -3.097275023406871775, 33.65873331764755250 ) ) ;
#2181 = DIRECTION ( 'NONE',  ( 0.000000000000000000, 0.000000000000000000, -1.000000000000000000 ) ) ;
#2182 = ORIENTED_EDGE ( 'NONE', *, *, #158, .T. ) ;
#2183 = DIRECTION ( 'NONE',  ( 1.000000000000000000, -0.000000000000000000, -0.000000000000000000 ) ) ;
#2184 = CARTESIAN_POINT ( 'NONE',  ( -13.05597421245628098, -5.800571792974073659, 36.04450365193367389 ) ) ;
#2185 = DIRECTION ( 'NONE',  ( -1.000000000000000000, 1.076498916035107744E-16, 0.000000000000000000 ) ) ;
#2186 = EDGE_CURVE ( 'NONE', #2774, #563, #4078, .T. ) ;
#2187 = AXIS2_PLACEMENT_3D ( 'NONE', #1766, #294, #4628 ) ;
#2188 = VERTEX_POINT ( 'NONE', #905 ) ;
#2189 = ORIENTED_EDGE ( 'NONE', *, *, #3783, .F. ) ;
#2190 = EDGE_CURVE ( 'NONE', #919, #2774, #2284, .T. ) ;
#2191 = EDGE_LOOP ( 'NONE', ( #214, #2719, #4191 ) ) ;
#2192 = EDGE_CURVE ( 'NONE', #3808, #2867, #1282, .T. ) ;
#2193 = EDGE_LOOP ( 'NONE', ( #2582, #1929 ) ) ;
#2194 = CARTESIAN_POINT ( 'NONE',  ( 13.83333314027810523, -3.573749167952788408, 32.36596039353566567 ) ) ;
#2195 = DIRECTION ( 'NONE',  ( 0.9999999999999998890, 5.286985906760955559E-16, 1.175275670495836481E-16 ) ) ;
#2196 = CARTESIAN_POINT ( 'NONE',  ( -12.02323308010481107, 7.719129963227447710, 17.66658805193229753 ) ) ;
#2197 = CARTESIAN_POINT ( 'NONE',  ( -12.87887028452541749, 6.192547044564507885, 35.96503381882250494 ) ) ;
#2198 = CARTESIAN_POINT ( 'NONE',  ( 14.28750723456195537, 0.4850620214986993139, 39.01512445358908820 ) ) ;
#2199 = CARTESIAN_POINT ( 'NONE',  ( 14.00291886944279973, -2.840536506667706629, 30.18479712748602140 ) ) ;
#2200 = CARTESIAN_POINT ( 'NONE',  ( -13.83332312227014604, -3.573749167952787076, 32.13020424815260867 ) ) ;
#2201 = MECHANICAL_DESIGN_GEOMETRIC_PRESENTATION_REPRESENTATION (  '', ( #1237 ), #4080 ) ;
#2202 = CARTESIAN_POINT ( 'NONE',  ( 5.009003980371977336E-06, 8.320472128100606877E-07, 17.65096039353565160 ) ) ;
#2203 = CARTESIAN_POINT ( 'NONE',  ( -7.619992765438047044, -6.393402013451324528, 17.90262445358908039 ) ) ;
#2204 = CARTESIAN_POINT ( 'NONE',  ( -13.83934412749958121, -3.546568056405964064, 32.33580404679898379 ) ) ;
#2205 = AXIS2_PLACEMENT_3D ( 'NONE', #306, #2386, #970 ) ;
#2206 = EDGE_CURVE ( 'NONE', #3396, #4255, #1156, .T. ) ;
#2207 = ORIENTED_EDGE ( 'NONE', *, *, #1799, .T. ) ;
#2208 = CYLINDRICAL_SURFACE ( 'NONE', #1797, 0.7500000000000006661 ) ;
#2209 = CARTESIAN_POINT ( 'NONE',  ( 6.870005009003977925, 12.08587093932537826, 18.40096039353565160 ) ) ;
#2210 = CARTESIAN_POINT ( 'NONE',  ( -4.762492765438045339, 0.004097986548673111795, -8.542375546410942988 ) ) ;
#2211 = ADVANCED_FACE ( 'NONE', ( #1246 ), #410, .T. ) ;
#2212 = VERTEX_POINT ( 'NONE', #1854 ) ;
#2213 = EDGE_LOOP ( 'NONE', ( #2250, #3855 ) ) ;
#2214 = CARTESIAN_POINT ( 'NONE',  ( -12.58714829887031073, 6.764457034226218468, 34.20002532364928527 ) ) ;
#2215 = ORIENTED_EDGE ( 'NONE', *, *, #1375, .F. ) ;
#2216 = ADVANCED_FACE ( 'NONE', ( #3287, #1271 ), #1993, .F. ) ;
#2217 = CYLINDRICAL_SURFACE ( 'NONE', #4271, 0.7499999999999997780 ) ;
#2218 = CARTESIAN_POINT ( 'NONE',  ( -13.83332312227014249, -3.573749167952786632, 32.36596039353566567 ) ) ;
#2219 = CARTESIAN_POINT ( 'NONE',  ( 3.750005009003979595, 8.320472128100606877E-07, 17.65096039353565160 ) ) ;
#2220 = CIRCLE ( 'NONE', #2436, 0.7500000000000006661 ) ;
#2221 = DIRECTION ( 'NONE',  ( -1.000000000000000000, 1.076498916035107744E-16, 0.000000000000000000 ) ) ;
#2222 = LINE ( 'NONE', #1464, #2594 ) ;
#2223 = CARTESIAN_POINT ( 'NONE',  ( 12.37117936981251987, 7.151597986548668295, 17.90262445358908039 ) ) ;
#2224 = FACE_OUTER_BOUND ( 'NONE', #1241, .T. ) ;
#2225 = LINE ( 'NONE', #1486, #2894 ) ;
#2226 = CIRCLE ( 'NONE', #352, 0.7499999999999997780 ) ;
#2227 = VERTEX_POINT ( 'NONE', #201 ) ;
#2228 = DIRECTION ( 'NONE',  ( 0.000000000000000000, 0.000000000000000000, 1.000000000000000000 ) ) ;
#2229 = CIRCLE ( 'NONE', #960, 3.573749999999999538 ) ;
#2230 = SPHERICAL_SURFACE ( 'NONE', #232, 0.5000000000000000000 ) ;
#2231 = FACE_OUTER_BOUND ( 'NONE', #3444, .T. ) ;
#2232 = ORIENTED_EDGE ( 'NONE', *, *, #72, .F. ) ;
#2233 = CARTESIAN_POINT ( 'NONE',  ( 12.37117714425454373, 7.897500832047208874, 17.65096039353565160 ) ) ;
#2234 = ORIENTED_EDGE ( 'NONE', *, *, #4225, .F. ) ;
#2235 = AXIS2_PLACEMENT_3D ( 'NONE', #830, #374, #1818 ) ;
#2236 = DIRECTION ( 'NONE',  ( 0.000000000000000000, 0.000000000000000000, 1.000000000000000000 ) ) ;
#2237 = ORIENTED_EDGE ( 'NONE', *, *, #4567, .F. ) ;
#2238 = ORIENTED_EDGE ( 'NONE', *, *, #1349, .F. ) ;
#2239 = CYLINDRICAL_SURFACE ( 'NONE', #2458, 3.573749999999998650 ) ;
#2240 = CARTESIAN_POINT ( 'NONE',  ( -13.66252080843872108, 4.184298707019366681, 38.16530575332425457 ) ) ;
#2241 = AXIS2_PLACEMENT_3D ( 'NONE', #1311, #585, #215 ) ;
#2242 = ADVANCED_FACE ( 'NONE', ( #2689 ), #1650, .F. ) ;
#2243 = DIRECTION ( 'NONE',  ( 0.000000000000000000, -1.000000000000000000, 0.000000000000000000 ) ) ;
#2244 = APPLICATION_CONTEXT ( 'automotive_design' ) ;
#2245 = VERTEX_POINT ( 'NONE', #3475 ) ;
#2246 = DIRECTION ( 'NONE',  ( -2.312964634635740689E-15, 0.000000000000000000, -1.000000000000000000 ) ) ;
#2247 = DIRECTION ( 'NONE',  ( 0.000000000000000000, 0.000000000000000000, 1.000000000000000000 ) ) ;
#2248 = CARTESIAN_POINT ( 'NONE',  ( 13.86272605794495405, -3.454216419310585540, 32.79868223278693762 ) ) ;
#2249 = DIRECTION ( 'NONE',  ( -1.000000000000000000, 0.000000000000000000, -0.000000000000000000 ) ) ;
#2250 = ORIENTED_EDGE ( 'NONE', *, *, #1376, .F. ) ;
#2251 = DIRECTION ( 'NONE',  ( 0.000000000000000000, -1.000000000000000000, 0.000000000000000000 ) ) ;
#2252 = CARTESIAN_POINT ( 'NONE',  ( -13.93157240826945475, -3.195140614832279624, 38.27608545593862033 ) ) ;
#2253 = AXIS2_PLACEMENT_3D ( 'NONE', #1056, #715, #2177 ) ;
#2254 = ORIENTED_EDGE ( 'NONE', *, *, #2471, .T. ) ;
#2255 = CARTESIAN_POINT ( 'NONE',  ( -8.369992765438043492, 7.151597986548673624, 17.90262445358908039 ) ) ;
#2256 = CARTESIAN_POINT ( 'NONE',  ( -17.48249499099600968, -7.147499167952783061, 32.36596039353565857 ) ) ;
#2257 = COLOUR_RGB ( '', 0.72549020, 0.75294118, 0.79215686) ;
#2258 = ADVANCED_FACE ( 'NONE', ( #246 ), #1111, .F. ) ;
#2259 = VERTEX_POINT ( 'NONE', #881 ) ;
#2260 = VERTEX_POINT ( 'NONE', #4510 ) ;
#2261 = CONTEXT_DEPENDENT_SHAPE_REPRESENTATION ( #3924, #596 ) ;
#2262 = DIRECTION ( 'NONE',  ( 0.000000000000000000, 0.000000000000000000, 1.000000000000000000 ) ) ;
#2263 = DIRECTION ( 'NONE',  ( -1.000000000000000000, 0.000000000000000000, 0.000000000000000000 ) ) ;
#2264 = ORIENTED_EDGE ( 'NONE', *, *, #3944, .T. ) ;
#2265 = CARTESIAN_POINT ( 'NONE',  ( -12.39928141451404997, 7.099434970714632698, 33.31939447329315129 ) ) ;
#2266 = VECTOR ( 'NONE', #4065, 1000.000000000000000 ) ;
#2267 = ADVANCED_FACE ( 'NONE', ( #1694 ), #2712, .T. ) ;
#2268 = CARTESIAN_POINT ( 'NONE',  ( 7.234561953626996335E-06, 0.004097986548672528061, 17.15262445358908039 ) ) ;
#2269 = EDGE_CURVE ( 'NONE', #719, #3403, #1221, .T. ) ;
#2270 = CARTESIAN_POINT ( 'NONE',  ( -12.30737424917090195, 7.261058540042763632, 17.49889617799752983 ) ) ;
#2271 = DIRECTION ( 'NONE',  ( -0.000000000000000000, -0.000000000000000000, -1.000000000000000000 ) ) ;
#2272 = CARTESIAN_POINT ( 'NONE',  ( -12.13298321006529790, 7.545450160427720654, 17.73224578507567628 ) ) ;
#2273 = EDGE_CURVE ( 'NONE', #4004, #2998, #2125, .T. ) ;
#2274 = ORIENTED_EDGE ( 'NONE', *, *, #4608, .F. ) ;
#2275 = DIRECTION ( 'NONE',  ( 9.517981353260378315E-33, 8.841607930564763213E-17, -1.000000000000000000 ) ) ;
#2276 = CARTESIAN_POINT ( 'NONE',  ( 13.83944209648124080, 3.554443468061219580, 31.39667678951239083 ) ) ;
#2277 = DIRECTION ( 'NONE',  ( 1.000000000000000000, 0.000000000000000000, 0.000000000000000000 ) ) ;
#2278 = AXIS2_PLACEMENT_3D ( 'NONE', #70, #321, #1029 ) ;
#2279 = EDGE_LOOP ( 'NONE', ( #1978, #1493, #2411, #133 ) ) ;
#2280 = DIRECTION ( 'NONE',  ( 0.000000000000000000, 0.000000000000000000, 1.000000000000000000 ) ) ;
#2281 = CARTESIAN_POINT ( 'NONE',  ( 3.262507234561983438, 0.004097986548672528061, -10.04237554641092345 ) ) ;
#2282 = ORIENTED_EDGE ( 'NONE', *, *, #3709, .T. ) ;
#2283 = CONTEXT_DEPENDENT_SHAPE_REPRESENTATION ( #2722, #562 ) ;
#2284 = LINE ( 'NONE', #197, #4029 ) ;
#2285 = LINE ( 'NONE', #1989, #3477 ) ;
#2286 = ORIENTED_EDGE ( 'NONE', *, *, #963, .T. ) ;
#2287 = CARTESIAN_POINT ( 'NONE',  ( 12.02320382733283743, 7.723282363347554913, 17.16832378532597758 ) ) ;
#2288 = CARTESIAN_POINT ( 'NONE',  ( 14.99250500900397753, 8.320472111961197689E-07, 32.36596039353565857 ) ) ;
#2289 = CARTESIAN_POINT ( 'NONE',  ( -3.749999999999999556, -3.750000000000000888, 146.2500000000000000 ) ) ;
#2290 = LINE ( 'NONE', #3431, #3543 ) ;
#2291 = ORIENTED_EDGE ( 'NONE', *, *, #828, .T. ) ;
#2292 = PLANE ( 'NONE',  #2020 ) ;
#2293 = DIRECTION ( 'NONE',  ( -1.000000000000000000, 1.076498916035107744E-16, 0.000000000000000000 ) ) ;
#2294 = DIRECTION ( 'NONE',  ( 0.000000000000000000, 0.000000000000000000, -1.000000000000000000 ) ) ;
#2295 = ORIENTED_EDGE ( 'NONE', *, *, #381, .T. ) ;
#2296 = CARTESIAN_POINT ( 'NONE',  ( 13.86256790811323469, -3.454845676089625339, 30.93920252718416819 ) ) ;
#2297 = B_SPLINE_CURVE_WITH_KNOTS ( 'NONE', 3,
 ( #3190, #4534, #2831, #1051, #689, #80, #2942, #2199, #1853, #1503, #3676, #3213, #1078, #710, #1811, #3233, #1461, #1465 ),
 .UNSPECIFIED., .F., .F.,
 ( 4, 2, 2, 2, 2, 2, 2, 2, 4 ),
 ( 0.000000000000000000, 0.0007012932024186013802, 0.001402586404837202760, 0.002103879607255804141, 0.002805172809674405521, 0.003506466012093006901, 0.004207759214511608281, 0.004909052416930209661, 0.005610345619348811042 ),
 .UNSPECIFIED. ) ;
#2298 = CYLINDRICAL_SURFACE ( 'NONE', #681, 0.7500000000000006661 ) ;
#2299 = VERTEX_POINT ( 'NONE', #2934 ) ;
#2300 = ORIENTED_EDGE ( 'NONE', *, *, #643, .T. ) ;
#2301 = CARTESIAN_POINT ( 'NONE',  ( 7.234561953626996335E-06, -3.565902013451327068, -1.469875546410923661 ) ) ;
#2302 = CIRCLE ( 'NONE', #1571, 3.573749999999998650 ) ;
#2303 = ADVANCED_FACE ( 'NONE', ( #2418 ), #3540, .T. ) ;
#2304 = VERTEX_POINT ( 'NONE', #1019 ) ;
#2305 = ADVANCED_FACE ( 'NONE', ( #1736 ), #3207, .T. ) ;
#2306 = VECTOR ( 'NONE', #1478, 1000.000000000000000 ) ;
#2307 = FACE_OUTER_BOUND ( 'NONE', #2955, .T. ) ;
#2308 = ADVANCED_FACE ( 'NONE', ( #795 ), #3515, .F. ) ;
#2309 = CARTESIAN_POINT ( 'NONE',  ( 17.28000050552179445, -3.039999999999999591, 17.78000050552179445 ) ) ;
#2310 = CARTESIAN_POINT ( 'NONE',  ( 13.60392201806077495, 4.370505649930263914, 38.02622764783904330 ) ) ;
#2311 = LINE ( 'NONE', #2667, #386 ) ;
#2312 = DIRECTION ( 'NONE',  ( 1.000000000000000000, -1.076498916035107621E-16, 0.000000000000000000 ) ) ;
#2313 = ORIENTED_EDGE ( 'NONE', *, *, #2529, .T. ) ;
#2314 = AXIS2_PLACEMENT_3D ( 'NONE', #2288, #506, #3705 ) ;
#2315 = DIRECTION ( 'NONE',  ( -1.000000000000000000, 1.076498916035107744E-16, -0.000000000000000000 ) ) ;
#2316 = DIRECTION ( 'NONE',  ( 1.000000000000000000, -8.673617379884035472E-17, 0.000000000000000000 ) ) ;
#2317 = ORIENTED_EDGE ( 'NONE', *, *, #3658, .F. ) ;
#2318 = SPHERICAL_SURFACE ( 'NONE', #2163, 0.5000000000000000000 ) ;
#2319 = CYLINDRICAL_SURFACE ( 'NONE', #4143, 3.573750000000000426 ) ;
#2320 = AXIS2_PLACEMENT_3D ( 'NONE', #1417, #2836, #3103 ) ;
#2321 = EDGE_CURVE ( 'NONE', #4454, #1623, #4257, .T. ) ;
#2322 = ORIENTED_EDGE ( 'NONE', *, *, #260, .T. ) ;
#2323 = ORIENTED_EDGE ( 'NONE', *, *, #2122, .T. ) ;
#2324 = CARTESIAN_POINT ( 'NONE',  ( -14.28749499099602005, 0.4808415968314561639, 39.51346039353565942 ) ) ;
#2325 = CARTESIAN_POINT ( 'NONE',  ( 12.37117714425454551, -7.147499167952786614, 32.36596039353565857 ) ) ;
#2326 = CIRCLE ( 'NONE', #2398, 0.7500000000000006661 ) ;
#2327 = EDGE_CURVE ( 'NONE', #563, #1729, #2226, .T. ) ;
#2328 = CIRCLE ( 'NONE', #4369, 7.147499999999999076 ) ;
#2329 = EDGE_CURVE ( 'NONE', #2845, #2188, #422, .T. ) ;
#2330 = B_SPLINE_CURVE_WITH_KNOTS ( 'NONE', 3,
 ( #2045, #1370, #2786, #4224, #1003, #208, #3074, #3867, #3525, #4516, #1304, #2718, #4160, #580, #3459, #227 ),
 .UNSPECIFIED., .F., .F.,
 ( 4, 2, 2, 2, 2, 2, 2, 4 ),
 ( 0.01121786453620356172, 0.01261999568898472708, 0.01332106126537531063, 0.01402212684176589418, 0.01472319241815647772, 0.01542425799454706301, 0.01612532357093764482, 0.01682638914732823010 ),
 .UNSPECIFIED. ) ;
#2331 = CIRCLE ( 'NONE', #3836, 0.5000000000000000000 ) ;
#2332 = ORIENTED_EDGE ( 'NONE', *, *, #3005, .F. ) ;
#2333 = DIRECTION ( 'NONE',  ( 0.000000000000000000, 0.000000000000000000, 1.000000000000000000 ) ) ;
#2334 = CARTESIAN_POINT ( 'NONE',  ( 8.370007234561949616, 7.901597986548672736, 17.15262445358908039 ) ) ;
#2335 = CARTESIAN_POINT ( 'NONE',  ( 13.05598645602221808, 5.804670611569964223, 36.54283959188025221 ) ) ;
#2336 = PLANE ( 'NONE',  #2634 ) ;
#2337 = ORIENTED_EDGE ( 'NONE', *, *, #259, .F. ) ;
#2338 = DIRECTION ( 'NONE',  ( 0.000000000000000000, 1.000000000000000000, 0.000000000000000000 ) ) ;
#2339 = ORIENTED_EDGE ( 'NONE', *, *, #810, .F. ) ;
#2340 = DIRECTION ( 'NONE',  ( 9.517981353260378315E-33, -8.841607930564763213E-17, 1.000000000000000000 ) ) ;
#2341 = EDGE_LOOP ( 'NONE', ( #2000, #3463, #2980, #2388 ) ) ;
#2342 = CYLINDRICAL_SURFACE ( 'NONE', #136, 0.5000000000000004441 ) ;
#2343 = CIRCLE ( 'NONE', #2130, 0.5000000000000000000 ) ;
#2344 = LINE ( 'NONE', #2093, #1193 ) ;
#2345 = ORIENTED_EDGE ( 'NONE', *, *, #773, .F. ) ;
#2346 = EDGE_CURVE ( 'NONE', #1947, #719, #3163, .T. ) ;
#2347 = ORIENTED_EDGE ( 'NONE', *, *, #3428, .T. ) ;
#2348 = UNCERTAINTY_MEASURE_WITH_UNIT (LENGTH_MEASURE( 1.000000000000000082E-05 ), #740, 'distance_accuracy_value', 'NONE');
#2349 = ORIENTED_EDGE ( 'NONE', *, *, #2409, .T. ) ;
#2350 = CARTESIAN_POINT ( 'NONE',  ( 3.040000505521796015, -3.039999999999999591, 3.040000505521796015 ) ) ;
#2351 = DIRECTION ( 'NONE',  ( 1.000000000000000000, 0.000000000000000000, 0.000000000000000000 ) ) ;
#2352 = SPHERICAL_SURFACE ( 'NONE', #2385, 0.5000000000000000000 ) ;
#2353 = CARTESIAN_POINT ( 'NONE',  ( 14.19373587001559933, 1.650820511743084307, 39.32424842390233266 ) ) ;
#2354 = DIRECTION ( 'NONE',  ( 0.000000000000000000, -0.000000000000000000, 1.000000000000000000 ) ) ;
#2355 = CARTESIAN_POINT ( 'NONE',  ( -17.48249499099600968, -7.147499167952782173, 3.790960393535648176 ) ) ;
#2356 = CARTESIAN_POINT ( 'NONE',  ( 13.94778095975370569, -3.099991964203534955, 34.15945326479446464 ) ) ;
#2357 = ORIENTED_EDGE ( 'NONE', *, *, #2075, .T. ) ;
#2358 = DIRECTION ( 'NONE',  ( 1.000000000000000000, 0.000000000000000000, 0.000000000000000000 ) ) ;
#2359 = VERTEX_POINT ( 'NONE', #3860 ) ;
#2360 = DIRECTION ( 'NONE',  ( 1.000000000000000000, 0.000000000000000000, 0.000000000000000000 ) ) ;
#2361 = AXIS2_PLACEMENT_3D ( 'NONE', #3453, #1388, #3093 ) ;
#2362 = PRODUCT_RELATED_PRODUCT_CATEGORY ( 'part', '', ( #611 ) ) ;
#2363 = VERTEX_POINT ( 'NONE', #2489 ) ;
#2364 = VECTOR ( 'NONE', #1326, 1000.000000000000000 ) ;
#2365 = CARTESIAN_POINT ( 'NONE',  ( 7.620005009003980589, -6.397499167952788390, 32.36596039353565857 ) ) ;
#2366 = CARTESIAN_POINT ( 'NONE',  ( -14.28749499099602005, 8.320472128100606877E-07, 17.65096039353565160 ) ) ;
#2367 = EDGE_LOOP ( 'NONE', ( #1231, #3132 ) ) ;
#2368 = VERTEX_POINT ( 'NONE', #4621 ) ;
#2369 = AXIS2_PLACEMENT_3D ( 'NONE', #1927, #4061, #4159 ) ;
#2370 = CARTESIAN_POINT ( 'NONE',  ( 10.16000050552179701, -6.586249999999999716, 10.16000050552179701 ) ) ;
#2371 = VECTOR ( 'NONE', #1970, 1000.000000000000000 ) ;
#2372 = VERTEX_POINT ( 'NONE', #74 ) ;
#2373 = CARTESIAN_POINT ( 'NONE',  ( 14.28750500900398279, 8.320472145597748469E-07, 28.79221039353566880 ) ) ;
#2374 = ADVANCED_FACE ( 'NONE', ( #3933 ), #1407, .T. ) ;
#2375 = CARTESIAN_POINT ( 'NONE',  ( 0.000000000000000000, 0.000000000000000000, 0.000000000000000000 ) ) ;
#2376 = CARTESIAN_POINT ( 'NONE',  ( -14.20052797712670767, -1.588767894053844554, 35.57559508471577914 ) ) ;
#2377 = CIRCLE ( 'NONE', #213, 1.499999999999999556 ) ;
#2378 = CYLINDRICAL_SURFACE ( 'NONE', #1444, 14.28750000000000142 ) ;
#2379 = CARTESIAN_POINT ( 'NONE',  ( 14.09186599505832405, -2.362174669806939686, 35.05771999556577612 ) ) ;
#2380 = DIRECTION ( 'NONE',  ( -0.000000000000000000, -0.000000000000000000, -1.000000000000000000 ) ) ;
#2381 = ORIENTED_EDGE ( 'NONE', *, *, #4354, .F. ) ;
#2382 = FACE_OUTER_BOUND ( 'NONE', #896, .T. ) ;
#2383 = ORIENTED_EDGE ( 'NONE', *, *, #1098, .T. ) ;
#2384 = CARTESIAN_POINT ( 'NONE',  ( 8.370005009003978813, 6.397500832047211539, 18.40096039353565160 ) ) ;
#2385 = AXIS2_PLACEMENT_3D ( 'NONE', #3519, #3797, #1324 ) ;
#2386 = DIRECTION ( 'NONE',  ( 0.000000000000000000, -1.000000000000000000, 0.000000000000000000 ) ) ;
#2387 =( BOUNDED_CURVE ( )  B_SPLINE_CURVE ( 3, ( #1562, #139, #869, #4403 ),
 .UNSPECIFIED., .F., .T. ) 
 B_SPLINE_CURVE_WITH_KNOTS ( ( 4, 4 ),
 ( 1.570796326794896558, 3.141592653589793116 ),
 .UNSPECIFIED. ) 
 CURVE ( )  GEOMETRIC_REPRESENTATION_ITEM ( )  RATIONAL_B_SPLINE_CURVE ( ( 1.000000000000000000, 0.8047378541243649375, 0.8047378541243649375, 1.000000000000000000 ) ) 
 REPRESENTATION_ITEM ( '' )  );
#2388 = ORIENTED_EDGE ( 'NONE', *, *, #961, .T. ) ;
#2389 = ORIENTED_EDGE ( 'NONE', *, *, #4619, .F. ) ;
#2390 = CARTESIAN_POINT ( 'NONE',  ( -3.152215195724335839, -3.565902013451327068, -8.542375546410942988 ) ) ;
#2391 = ADVANCED_FACE ( 'NONE', ( #2144 ), #3322, .F. ) ;
#2392 = ORIENTED_EDGE ( 'NONE', *, *, #748, .T. ) ;
#2393 = CARTESIAN_POINT ( 'NONE',  ( 2.540000505521796015, -17.78000000000000114, 17.28000050552179445 ) ) ;
#2394 = CARTESIAN_POINT ( 'NONE',  ( -13.93157463382742378, -3.199237769333737713, 38.77442139588517733 ) ) ;
#2395 = FACE_OUTER_BOUND ( 'NONE', #3275, .T. ) ;
#2396 = DIRECTION ( 'NONE',  ( 0.000000000000000000, 0.000000000000000000, 1.000000000000000000 ) ) ;
#2397 = CIRCLE ( 'NONE', #3393, 3.573749999999998650 ) ;
#2398 = AXIS2_PLACEMENT_3D ( 'NONE', #3168, #1510, #2925 ) ;
#2399 = VECTOR ( 'NONE', #595, 1000.000000000000000 ) ;
#2400 = ADVANCED_FACE ( 'NONE', ( #2775 ), #1385, .T. ) ;
#2401 = EDGE_CURVE ( 'NONE', #2299, #952, #2673, .T. ) ;
#2402 = CARTESIAN_POINT ( 'NONE',  ( 13.88012347307862449, -3.388720364211946556, 33.52461916018275190 ) ) ;
#2403 = PRODUCT ( 'MAS-681', 'MAS-681', '', ( #2147 ) ) ;
#2404 = FACE_OUTER_BOUND ( 'NONE', #443, .T. ) ;
#2405 = ORIENTED_EDGE ( 'NONE', *, *, #1440, .T. ) ;
#2406 = DIRECTION ( 'NONE',  ( -0.000000000000000000, -0.000000000000000000, -1.000000000000000000 ) ) ;
#2407 = VECTOR ( 'NONE', #3585, 1000.000000000000000 ) ;
#2408 = CARTESIAN_POINT ( 'NONE',  ( 11.90639614989969886, 7.897500832047208874, 17.65096039353565160 ) ) ;
#2409 = EDGE_CURVE ( 'NONE', #3774, #3954, #1712, .T. ) ;
#2410 = ADVANCED_FACE ( 'NONE', ( #843 ), #3715, .F. ) ;
#2411 = ORIENTED_EDGE ( 'NONE', *, *, #456, .T. ) ;
#2412 = CARTESIAN_POINT ( 'NONE',  ( -13.83332312227014427, 3.573750832047213777, 32.36596039353566567 ) ) ;
#2413 = CARTESIAN_POINT ( 'NONE',  ( 2.316727177394501718E-17, 0.000000000000000000, 4.762500000000001066 ) ) ;
#2414 = ORIENTED_EDGE ( 'NONE', *, *, #1281, .T. ) ;
#2415 = PRESENTATION_LAYER_ASSIGNMENT (  '', '', ( #3410 ) ) ;
#2416 = EDGE_LOOP ( 'NONE', ( #3370, #1036, #4111, #927 ) ) ;
#2417 = ORIENTED_EDGE ( 'NONE', *, *, #743, .T. ) ;
#2418 = FACE_OUTER_BOUND ( 'NONE', #4618, .T. ) ;
#2419 = DIRECTION ( 'NONE',  ( -1.000000000000000000, 0.000000000000000000, 0.000000000000000000 ) ) ;
#2420 = SHAPE_REPRESENTATION_RELATIONSHIP ( 'NONE' , 'NONE' ,  #2796, #3970 ) ;
#2421 = DIRECTION ( 'NONE',  ( -1.000000000000000000, 1.776412614630121196E-15, 0.000000000000000000 ) ) ;
#2422 = CARTESIAN_POINT ( 'NONE',  ( 12.62992674139356097, -6.680416156580533560, 34.91794089097076892 ) ) ;
#2423 = DIRECTION ( 'NONE',  ( 0.000000000000000000, 0.000000000000000000, 1.000000000000000000 ) ) ;
#2424 = CARTESIAN_POINT ( 'NONE',  ( 14.17613779523199291, -1.791259416094247880, 35.46724785073431008 ) ) ;
#2425 = CARTESIAN_POINT ( 'NONE',  ( -12.37116712624658454, 7.147500832047209762, 17.65096039353565160 ) ) ;
#2426 = CARTESIAN_POINT ( 'NONE',  ( 8.370005009003978813, -7.147499167952784838, 17.65096039353565160 ) ) ;
#2427 = DIRECTION ( 'NONE',  ( 0.000000000000000000, 0.000000000000000000, 1.000000000000000000 ) ) ;
#2428 = ADVANCED_FACE ( 'NONE', ( #4096 ), #3365, .T. ) ;
#2429 = ORIENTED_EDGE ( 'NONE', *, *, #1855, .T. ) ;
#2430 = CARTESIAN_POINT ( 'NONE',  ( -3.573749999999998650, 0.000000000000000000, 33.33750000000000568 ) ) ;
#2431 = AXIS2_PLACEMENT_3D ( 'NONE', #2830, #4624, #4291 ) ;
#2432 = EDGE_CURVE ( 'NONE', #4095, #3460, #2387, .T. ) ;
#2433 = CARTESIAN_POINT ( 'NONE',  ( 7.234561953626996335E-06, 0.004097986548672528061, 17.15262445358908039 ) ) ;
#2434 = CARTESIAN_POINT ( 'NONE',  ( 8.370007234561953169, -6.393402013451326305, 31.86762445358908735 ) ) ;
#2435 = CIRCLE ( 'NONE', #3870, 14.28750000000000142 ) ;
#2436 = AXIS2_PLACEMENT_3D ( 'NONE', #4537, #2025, #3101 ) ;
#2437 = VERTEX_POINT ( 'NONE', #2255 ) ;
#2438 = EDGE_LOOP ( 'NONE', ( #615, #1059, #4266, #2802 ) ) ;
#2439 = LINE ( 'NONE', #617, #579 ) ;
#2440 = AXIS2_PLACEMENT_3D ( 'NONE', #1888, #288, #3560 ) ;
#2441 = PRODUCT_DEFINITION_SHAPE ( 'NONE', 'NONE',  #3981 ) ;
#2442 = ORIENTED_EDGE ( 'NONE', *, *, #4127, .F. ) ;
#2443 = CARTESIAN_POINT ( 'NONE',  ( 12.18303574196747263, 7.464156020238631228, 17.78097603577003127 ) ) ;
#2444 = EDGE_LOOP ( 'NONE', ( #4386, #2274 ) ) ;
#2445 = CARTESIAN_POINT ( 'NONE',  ( -13.86271173127319400, 3.462410270568636150, 30.93674631171511180 ) ) ;
#2446 = AXIS2_PLACEMENT_3D ( 'NONE', #2413, #3443, #2704 ) ;
#2447 = CARTESIAN_POINT ( 'NONE',  ( -13.83332312227014249, -3.573749167952786632, 32.36596039353566567 ) ) ;
#2448 = CARTESIAN_POINT ( 'NONE',  ( 14.10222980048032326, -2.335234415017074294, 39.13740046776372594 ) ) ;
#2449 = CARTESIAN_POINT ( 'NONE',  ( -8.369992765438043492, 7.901597986548672736, 17.90262445358908039 ) ) ;
#2450 = EDGE_CURVE ( 'NONE', #2014, #1208, #796, .T. ) ;
#2451 = LINE ( 'NONE', #252, #460 ) ;
#2452 = CARTESIAN_POINT ( 'NONE',  ( -12.27078712905513314, -7.318982076682964966, 17.91363472736961171 ) ) ;
#2453 = CIRCLE ( 'NONE', #4343, 3.573749999999999538 ) ;
#2454 = CARTESIAN_POINT ( 'NONE',  ( 17.78000050552179800, -17.78000000000000114, 3.040000505521795571 ) ) ;
#2455 = LINE ( 'NONE', #4562, #3765 ) ;
#2456 = ORIENTED_EDGE ( 'NONE', *, *, #3194, .F. ) ;
#2457 = CARTESIAN_POINT ( 'NONE',  ( 18.74250500900397753, -3.573749167952788852, 32.36596039353566567 ) ) ;
#2458 = AXIS2_PLACEMENT_3D ( 'NONE', #777, #55, #3305 ) ;
#2459 = CYLINDRICAL_SURFACE ( 'NONE', #1320, 3.573749999999999538 ) ;
#2460 = EDGE_LOOP ( 'NONE', ( #947, #3606 ) ) ;
#2461 = B_SPLINE_CURVE_WITH_KNOTS ( 'NONE', 3,
 ( #775, #380, #2844, #725, #2865, #4359, #2823, #2487, #3227, #2166, #2565, #4310, #1068, #2, #3930, #1451, #3605, #1042, #2214, #1825, #3646, #27, #1476, #1758 ),
 .UNSPECIFIED., .F., .F.,
 ( 4, 2, 2, 2, 2, 2, 2, 2, 2, 2, 2, 4 ),
 ( -1.301042606982605321E-18, 0.001420502804142392784, 0.002841005608284786869, 0.004261508412427179870, 0.004971759814498384611, 0.005682011216569587617, 0.006392262618640790622, 0.007102514020711995363, 0.008523016824854413517, 0.009233268226925623462, 0.009943519628996833407, 0.01136402243313923421 ),
 .UNSPECIFIED. ) ;
#2462 = ORIENTED_EDGE ( 'NONE', *, *, #1718, .T. ) ;
#2463 = AXIS2_PLACEMENT_3D ( 'NONE', #4270, #2737, #4581 ) ;
#2464 = VERTEX_POINT ( 'NONE', #3004 ) ;
#2465 = CARTESIAN_POINT ( 'NONE',  ( 12.30672194145874876, 7.258094028239606921, 17.99507373849869651 ) ) ;
#2466 = CARTESIAN_POINT ( 'NONE',  ( -13.83947098521712249, 3.554273134874391005, 31.39569820401975164 ) ) ;
#2467 = EDGE_CURVE ( 'NONE', #560, #4140, #1236, .T. ) ;
#2468 = PRODUCT_CONTEXT ( 'NONE', #1297, 'mechanical' ) ;
#2469 = CARTESIAN_POINT ( 'NONE',  ( 8.370005009003978813, -7.897499167952783949, 17.65096039353565160 ) ) ;
#2470 = CARTESIAN_POINT ( 'NONE',  ( 13.48425421428311211, -4.726822391962680392, 37.73224719609672917 ) ) ;
#2471 = EDGE_CURVE ( 'NONE', #3603, #567, #2696, .T. ) ;
#2472 = CIRCLE ( 'NONE', #451, 14.28750000000000142 ) ;
#2473 = CARTESIAN_POINT ( 'NONE',  ( 3.750000000000000000, 3.750000000000000000, 146.2500000000000000 ) ) ;
#2474 = LINE ( 'NONE', #11, #3992 ) ;
#2475 =( REPRESENTATION_RELATIONSHIP ('NONE','NONE', #4401, #3415 ) REPRESENTATION_RELATIONSHIP_WITH_TRANSFORMATION ( #1918 )SHAPE_REPRESENTATION_RELATIONSHIP( ) );
#2476 = DIRECTION ( 'NONE',  ( 1.707404996040164265E-16, -1.000000000000000000, 0.000000000000000000 ) ) ;
#2477 = LINE ( 'NONE', #3569, #4588 ) ;
#2478 = LINE ( 'NONE', #300, #1145 ) ;
#2479 = AXIS2_PLACEMENT_3D ( 'NONE', #3848, #1419, #629 ) ;
#2480 = AXIS2_PLACEMENT_3D ( 'NONE', #3524, #296, #1744 ) ;
#2481 = EDGE_LOOP ( 'NONE', ( #3602, #776, #379, #3416 ) ) ;
#2482 = CARTESIAN_POINT ( 'NONE',  ( 13.05555083129287652, -5.801549086471636585, 36.04312068514320799 ) ) ;
#2483 = CIRCLE ( 'NONE', #4296, 0.7499999999999997780 ) ;
#2484 = PLANE ( 'NONE',  #4540 ) ;
#2485 = EDGE_LOOP ( 'NONE', ( #1761, #3065, #1662, #3771, #1538 ) ) ;
#2486 = VERTEX_POINT ( 'NONE', #2525 ) ;
#2487 = CARTESIAN_POINT ( 'NONE',  ( -13.66251858288074850, 4.188395861520828767, 37.66696981337766914 ) ) ;
#2488 = ORIENTED_EDGE ( 'NONE', *, *, #4005, .F. ) ;
#2489 = CARTESIAN_POINT ( 'NONE',  ( 3.750005009003979595, -3.749999167952787538, 17.65096039353565160 ) ) ;
#2490 = EDGE_LOOP ( 'NONE', ( #124, #4062, #1018, #2238 ) ) ;
#2491 = CARTESIAN_POINT ( 'NONE',  ( 14.99250500900398109, 7.147500832047209762, 3.790960393535649064 ) ) ;
#2492 = CARTESIAN_POINT ( 'NONE',  ( 0.000000000000000000, 0.000000000000000000, 0.000000000000000000 ) ) ;
#2493 = CARTESIAN_POINT ( 'NONE',  ( -13.05553858772694120, 5.805647905067521819, 36.54145662508980053 ) ) ;
#2494 = CYLINDRICAL_SURFACE ( 'NONE', #4450, 0.5000000000000000000 ) ;
#2495 = AXIS2_PLACEMENT_3D ( 'NONE', #4380, #1166, #137 ) ;
#2496 = DIRECTION ( 'NONE',  ( -0.000000000000000000, -0.000000000000000000, 1.000000000000000000 ) ) ;
#2497 = DIRECTION ( 'NONE',  ( -1.076498916035107621E-16, 1.000000000000000000, -0.000000000000000000 ) ) ;
#2498 = DIRECTION ( 'NONE',  ( 0.000000000000000000, 0.000000000000000000, 1.000000000000000000 ) ) ;
#2499 = CYLINDRICAL_SURFACE ( 'NONE', #1730, 3.573750000000000426 ) ;
#2500 = DIRECTION ( 'NONE',  ( -1.000000000000000000, 1.076498916035107744E-16, 0.000000000000000000 ) ) ;
#2501 = ORIENTED_EDGE ( 'NONE', *, *, #4196, .F. ) ;
#2502 = CARTESIAN_POINT ( 'NONE',  ( 14.24247714116602737, 1.154283519900359600, 35.75635498855329786 ) ) ;
#2503 = CARTESIAN_POINT ( 'NONE',  ( -6.869992765438047932, -6.393402013451324528, 17.15262445358908039 ) ) ;
#2504 = EDGE_CURVE ( 'NONE', #2506, #3737, #1420, .T. ) ;
#2505 = DIRECTION ( 'NONE',  ( 0.000000000000000000, 0.000000000000000000, -1.000000000000000000 ) ) ;
#2506 = VERTEX_POINT ( 'NONE', #4038 ) ;
#2507 = ORIENTED_EDGE ( 'NONE', *, *, #547, .T. ) ;
#2508 = ADVANCED_FACE ( 'NONE', ( #2950, #3311 ), #742, .T. ) ;
#2509 =( GEOMETRIC_REPRESENTATION_CONTEXT ( 3 ) GLOBAL_UNCERTAINTY_ASSIGNED_CONTEXT ( ( #1990 ) ) GLOBAL_UNIT_ASSIGNED_CONTEXT ( ( #3935, #2569, #3563 ) ) REPRESENTATION_CONTEXT ( 'NONE', 'WORKASPACE' ) );
#2510 = EDGE_CURVE ( 'NONE', #1208, #2845, #1468, .T. ) ;
#2511 = ORIENTED_EDGE ( 'NONE', *, *, #2122, .F. ) ;
#2512 = EDGE_LOOP ( 'NONE', ( #2073, #2868, #3151, #2381, #1200 ) ) ;
#2513 = CARTESIAN_POINT ( 'NONE',  ( 3.749999999999999556, 3.750000000000000000, 18.74999999999999645 ) ) ;
#2514 = AXIS2_PLACEMENT_3D ( 'NONE', #2572, #1833, #3568 ) ;
#2515 = DIRECTION ( 'NONE',  ( 0.000000000000000000, 0.000000000000000000, 1.000000000000000000 ) ) ;
#2516 = LINE ( 'NONE', #4317, #3911 ) ;
#2517 = CARTESIAN_POINT ( 'NONE',  ( 14.26329643125615476, 0.9577320989239291871, 38.96707689327597279 ) ) ;
#2518 = CARTESIAN_POINT ( 'NONE',  ( -12.37116712624658810, -7.147499167952783061, 18.40096039353565160 ) ) ;
#2519 = ADVANCED_FACE ( 'NONE', ( #65 ), #43, .F. ) ;
#2520 = CARTESIAN_POINT ( 'NONE',  ( 3.152229664848242852, -3.565902013451327068, -8.542375546410942988 ) ) ;
#2521 = CARTESIAN_POINT ( 'NONE',  ( 4.762507234561953240, 0.004097986548672528061, -8.542375546410942988 ) ) ;
#2522 = PLANE ( 'NONE',  #818 ) ;
#2523 = VECTOR ( 'NONE', #2746, 1000.000000000000000 ) ;
#2524 = CARTESIAN_POINT ( 'NONE',  ( 14.24237798928296783, -1.151061070837056777, 35.25757041514634693 ) ) ;
#2525 = CARTESIAN_POINT ( 'NONE',  ( 4.762507234561953240, 0.004097986548672528061, 3.292624453589077405 ) ) ;
#2526 = EDGE_LOOP ( 'NONE', ( #2638, #4163, #1936, #2189 ) ) ;
#2527 = DIRECTION ( 'NONE',  ( -1.000000000000000000, 8.673617379884035472E-17, 0.000000000000000000 ) ) ;
#2528 = FACE_OUTER_BOUND ( 'NONE', #3649, .T. ) ;
#2529 = EDGE_CURVE ( 'NONE', #2975, #1428, #1028, .T. ) ;
#2530 = AXIS2_PLACEMENT_3D ( 'NONE', #186, #1907, #3340 ) ;
#2531 = EDGE_CURVE ( 'NONE', #3559, #1846, #2225, .T. ) ;
#2532 = CARTESIAN_POINT ( 'NONE',  ( 14.99250723456195544, 7.151597986548670072, 3.292624453589077405 ) ) ;
#2533 = AXIS2_PLACEMENT_3D ( 'NONE', #2803, #2102, #4289 ) ;
#2534 = ORIENTED_EDGE ( 'NONE', *, *, #2510, .T. ) ;
#2535 = EDGE_LOOP ( 'NONE', ( #2507, #1456, #3541, #4309 ) ) ;
#2536 =( NAMED_UNIT ( * ) PLANE_ANGLE_UNIT ( ) SI_UNIT ( $, .RADIAN. ) );
#2537 = ORIENTED_EDGE ( 'NONE', *, *, #3080, .F. ) ;
#2538 = ORIENTED_EDGE ( 'NONE', *, *, #734, .T. ) ;
#2539 = DIRECTION ( 'NONE',  ( 0.000000000000000000, 0.000000000000000000, 1.000000000000000000 ) ) ;
#2540 = APPLICATION_PROTOCOL_DEFINITION ( 'draft international standard', 'automotive_design', 1998, #3989 ) ;
#2541 = CARTESIAN_POINT ( 'NONE',  ( 2.193906090638697570, -3.565902013451327068, -9.141961161702393923 ) ) ;
#2542 = ADVANCED_FACE ( 'NONE', ( #3661 ), #89, .T. ) ;
#2543 =( BOUNDED_CURVE ( )  B_SPLINE_CURVE ( 3, ( #179, #4083, #432, #1224 ),
 .UNSPECIFIED., .F., .F. ) 
 B_SPLINE_CURVE_WITH_KNOTS ( ( 4, 4 ),
 ( 4.712388980384689674, 6.283185307179586232 ),
 .UNSPECIFIED. ) 
 CURVE ( )  GEOMETRIC_REPRESENTATION_ITEM ( )  RATIONAL_B_SPLINE_CURVE ( ( 1.000000000000000000, 0.8047378541243649375, 0.8047378541243649375, 1.000000000000000000 ) ) 
 REPRESENTATION_ITEM ( '' )  );
#2544 = FACE_OUTER_BOUND ( 'NONE', #921, .T. ) ;
#2545 = DIRECTION ( 'NONE',  ( 0.000000000000000000, 1.000000000000000000, 8.673617379884026597E-16 ) ) ;
#2546 = CARTESIAN_POINT ( 'NONE',  ( -12.37116712624658810, -7.147499167952783061, 18.40096039353565160 ) ) ;
#2547 = DIRECTION ( 'NONE',  ( 1.000000000000000000, -1.076498916035107744E-16, 0.000000000000000000 ) ) ;
#2548 = CIRCLE ( 'NONE', #907, 0.7500000000000006661 ) ;
#2549 = LINE ( 'NONE', #3993, #154 ) ;
#2550 = ADVANCED_FACE ( 'NONE', ( #2881 ), #4348, .T. ) ;
#2551 = LINE ( 'NONE', #3337, #354 ) ;
#2552 = EDGE_CURVE ( 'NONE', #1822, #3350, #2551, .T. ) ;
#2553 = AXIS2_PLACEMENT_3D ( 'NONE', #3147, #3617, #1160 ) ;
#2554 = ORIENTED_EDGE ( 'NONE', *, *, #448, .F. ) ;
#2555 = CARTESIAN_POINT ( 'NONE',  ( 17.78000050552179800, -17.28000000000000114, 3.040000505521795571 ) ) ;
#2556 = CARTESIAN_POINT ( 'NONE',  ( -14.19372362644966756, -1.646721693147197740, 38.82591248395577566 ) ) ;
#2557 = B_SPLINE_CURVE_WITH_KNOTS ( 'NONE', 3,
 ( #1860, #4037, #2204, #2948, #4416, #1815, #2180, #764, #392, #2574, #370, #4014, #1837, #3637, #4395, #3335, #435, #1182 ),
 .UNSPECIFIED., .F., .F.,
 ( 4, 2, 2, 2, 2, 2, 2, 2, 4 ),
 ( 0.01682638914732823010, 0.01752717873359116094, 0.01822796831985409177, 0.01892875790611702261, 0.01962954749237995344, 0.02033033707864288775, 0.02103112666490581859, 0.02173191625116874942, 0.02243270583743168026 ),
 .UNSPECIFIED. ) ;
#2558 = CIRCLE ( 'NONE', #1750, 0.5000000000000004441 ) ;
#2559 = B_SPLINE_CURVE_WITH_KNOTS ( 'NONE', 3,
 ( #4461, #1248, #2287, #2595, #1877, #3352, #1201, #3040, #2644, #151 ),
 .UNSPECIFIED., .F., .F.,
 ( 4, 2, 2, 2, 4 ),
 ( 0.000000000000000000, 0.0003186827706029870567, 0.0006373655412059741135, 0.0009560483118089611702, 0.001274731082411948227 ),
 .UNSPECIFIED. ) ;
#2560 = EDGE_CURVE ( 'NONE', #2910, #4543, #1342, .T. ) ;
#2561 =( GEOMETRIC_REPRESENTATION_CONTEXT ( 3 ) GLOBAL_UNCERTAINTY_ASSIGNED_CONTEXT ( ( #1292 ) ) GLOBAL_UNIT_ASSIGNED_CONTEXT ( ( #457, #858, #3724 ) ) REPRESENTATION_CONTEXT ( 'NONE', 'WORKASPACE' ) );
#2562 = DIRECTION ( 'NONE',  ( 0.000000000000000000, -1.000000000000000000, 0.000000000000000000 ) ) ;
#2563 = ORIENTED_EDGE ( 'NONE', *, *, #2954, .F. ) ;
#2564 = EDGE_LOOP ( 'NONE', ( #3607, #968 ) ) ;
#2565 = CARTESIAN_POINT ( 'NONE',  ( -13.42336662775846889, 4.900590130444159698, 37.07949484329716938 ) ) ;
#2566 = VERTEX_POINT ( 'NONE', #463 ) ;
#2567 = ORIENTED_EDGE ( 'NONE', *, *, #1923, .T. ) ;
#2568 = DIRECTION ( 'NONE',  ( -1.000000000000000000, 0.000000000000000000, 0.000000000000000000 ) ) ;
#2569 =( NAMED_UNIT ( * ) PLANE_ANGLE_UNIT ( ) SI_UNIT ( $, .RADIAN. ) );
#2570 = CARTESIAN_POINT ( 'NONE',  ( 13.30106093516862842, 5.223730645347358426, 36.75583910459432246 ) ) ;
#2571 = CARTESIAN_POINT ( 'NONE',  ( -13.87970016671034656, 3.390430244675832316, 31.21191674207121380 ) ) ;
#2572 = CARTESIAN_POINT ( 'NONE',  ( 7.620007234561951392, 12.08996809382683857, 39.01512445358908110 ) ) ;
#2573 = DIRECTION ( 'NONE',  ( -1.000000000000000000, 1.076498916035107621E-16, 0.000000000000000000 ) ) ;
#2574 = CARTESIAN_POINT ( 'NONE',  ( -14.09151203141540520, -2.360106401758869321, 34.55760183291916121 ) ) ;
#2575 = DIRECTION ( 'NONE',  ( -1.000000000000000000, 1.076498916035107621E-16, -0.000000000000000000 ) ) ;
#2576 = VECTOR ( 'NONE', #4470, 1000.000000000000000 ) ;
#2577 = DIRECTION ( 'NONE',  ( 0.000000000000000000, 0.000000000000000000, -1.000000000000000000 ) ) ;
#2578 = ORIENTED_EDGE ( 'NONE', *, *, #361, .T. ) ;
#2579 = DIRECTION ( 'NONE',  ( 0.000000000000000000, 0.000000000000000000, 1.000000000000000000 ) ) ;
#2580 = CARTESIAN_POINT ( 'NONE',  ( -13.83080859801392570, -3.601725888500601602, 38.05633745867910278 ) ) ;
#2581 = ADVANCED_FACE ( 'NONE', ( #786 ), #1904, .F. ) ;
#2582 = ORIENTED_EDGE ( 'NONE', *, *, #792, .T. ) ;
#2583 = DIRECTION ( 'NONE',  ( 0.000000000000000000, 0.000000000000000000, -1.000000000000000000 ) ) ;
#2584 = EDGE_CURVE ( 'NONE', #3907, #696, #1940, .T. ) ;
#2585 = DIRECTION ( 'NONE',  ( 0.000000000000000000, 0.000000000000000000, 1.000000000000000000 ) ) ;
#2586 = DIRECTION ( 'NONE',  ( -1.000000000000000000, -0.000000000000000000, -0.000000000000000000 ) ) ;
#2587 = CARTESIAN_POINT ( 'NONE',  ( 10.16000050552179701, -10.16000000000000014, 17.78000050552179445 ) ) ;
#2588 = ORIENTED_EDGE ( 'NONE', *, *, #57, .T. ) ;
#2589 = ORIENTED_EDGE ( 'NONE', *, *, #2327, .T. ) ;
#2590 = CARTESIAN_POINT ( 'NONE',  ( -14.17583154969198134, 1.793507453721278511, 35.46587530915064690 ) ) ;
#2591 = AXIS2_PLACEMENT_3D ( 'NONE', #2714, #666, #2103 ) ;
#2592 = DIRECTION ( 'NONE',  ( 0.000000000000000000, 0.000000000000000000, -1.000000000000000000 ) ) ;
#2593 = ORIENTED_EDGE ( 'NONE', *, *, #1621, .F. ) ;
#2594 = VECTOR ( 'NONE', #692, 1000.000000000000000 ) ;
#2595 = CARTESIAN_POINT ( 'NONE',  ( 12.13220700912610894, 7.550805373316674007, 17.23334239392282186 ) ) ;
#2596 = DIRECTION ( 'NONE',  ( 0.000000000000000000, 0.000000000000000000, -1.000000000000000000 ) ) ;
#2597 = DIRECTION ( 'NONE',  ( 1.000000000000000000, 0.000000000000000000, 0.000000000000000000 ) ) ;
#2598 = DIRECTION ( 'NONE',  ( 1.076498916035107621E-16, -1.000000000000000000, 0.000000000000000000 ) ) ;
#2599 = AXIS2_PLACEMENT_3D ( 'NONE', #929, #3908, #2583 ) ;
#2600 = ORIENTED_EDGE ( 'NONE', *, *, #1849, .F. ) ;
#2601 = CARTESIAN_POINT ( 'NONE',  ( 13.92222260900385855, 3.211378106144403777, 33.95122015944071592 ) ) ;
#2602 = CONICAL_SURFACE ( 'NONE', #1487, 3.262500000000029932, 0.7853981633974446153 ) ;
#2603 = FACE_OUTER_BOUND ( 'NONE', #2213, .T. ) ;
#2604 = CIRCLE ( 'NONE', #4034, 3.573749999999999538 ) ;
#2605 = ADVANCED_FACE ( 'NONE', ( #655, #2157 ), #206, .F. ) ;
#2606 = DIRECTION ( 'NONE',  ( -1.000000000000000000, 1.076498916035107744E-16, 0.000000000000000000 ) ) ;
#2607 = EDGE_LOOP ( 'NONE', ( #4326, #2300, #662, #2661 ) ) ;
#2608 = CARTESIAN_POINT ( 'NONE',  ( 3.040000505521795571, -17.28000000000000114, 3.040000505521795571 ) ) ;
#2609 = VECTOR ( 'NONE', #2315, 1000.000000000000000 ) ;
#2610 = LINE ( 'NONE', #4098, #3165 ) ;
#2611 = ADVANCED_FACE ( 'NONE', ( #1629 ), #3045, .F. ) ;
#2612 = EDGE_LOOP ( 'NONE', ( #2820, #588, #330, #1138 ) ) ;
#2613 = VERTEX_POINT ( 'NONE', #4515 ) ;
#2614 = CARTESIAN_POINT ( 'NONE',  ( 14.03228230178743097, 2.693715529912121820, 30.00579653744681252 ) ) ;
#2615 = CONICAL_SURFACE ( 'NONE', #892, 3.262500000000029932, 0.7853981633974446153 ) ;
#2616 = CARTESIAN_POINT ( 'NONE',  ( -12.37116490068861197, -7.143402013451321864, 17.90262445358908039 ) ) ;
#2617 = EDGE_LOOP ( 'NONE', ( #2911, #4643, #1795 ) ) ;
#2618 = EDGE_CURVE ( 'NONE', #971, #3225, #502, .T. ) ;
#2619 = DIRECTION ( 'NONE',  ( 0.000000000000000000, 0.000000000000000000, 1.000000000000000000 ) ) ;
#2620 = AXIS2_PLACEMENT_3D ( 'NONE', #1025, #2042, #2421 ) ;
#2621 = EDGE_CURVE ( 'NONE', #563, #2566, #2977, .T. ) ;
#2622 = DIRECTION ( 'NONE',  ( 1.000000000000000000, -1.076498916035107621E-16, -0.000000000000000000 ) ) ;
#2623 = CARTESIAN_POINT ( 'NONE',  ( 13.73375050552179566, -12.25345428146915161, 13.73375050552179566 ) ) ;
#2624 = CARTESIAN_POINT ( 'NONE',  ( -12.18356977001436370, 7.463263818241263614, 17.78165220884836728 ) ) ;
#2625 = DIRECTION ( 'NONE',  ( -1.076498916035107621E-16, -1.000000000000000000, -8.841607930564763213E-17 ) ) ;
#2626 = EDGE_LOOP ( 'NONE', ( #3787, #4019, #618, #3834 ) ) ;
#2627 = CYLINDRICAL_SURFACE ( 'NONE', #4419, 0.7499999999999997780 ) ;
#2628 = CARTESIAN_POINT ( 'NONE',  ( 8.370007234561949616, -7.143402013451325416, 17.15262445358908039 ) ) ;
#2629 = ORIENTED_EDGE ( 'NONE', *, *, #643, .F. ) ;
#2630 = DIRECTION ( 'NONE',  ( 0.000000000000000000, 0.000000000000000000, -1.000000000000000000 ) ) ;
#2631 = CARTESIAN_POINT ( 'NONE',  ( 13.73375050552179744, -10.16000000000000014, 6.586250505521794807 ) ) ;
#2632 = DIRECTION ( 'NONE',  ( -1.000000000000000000, 0.000000000000000000, 0.000000000000000000 ) ) ;
#2633 = AXIS2_PLACEMENT_3D ( 'NONE', #3588, #3548, #3193 ) ;
#2634 = AXIS2_PLACEMENT_3D ( 'NONE', #132, #535, #3728 ) ;
#2635 = B_SPLINE_CURVE_WITH_KNOTS ( 'NONE', 3,
 ( #121, #143, #822, #1264, #493, #3325, #1216, #4453, #1588, #3768, #2636, #546, #873, #2960, #3743, #847 ),
 .UNSPECIFIED., .F., .F.,
 ( 4, 2, 2, 2, 2, 2, 2, 4 ),
 ( 0.01121777374642162275, 0.01261988060185674498, 0.01332093402957430610, 0.01402198745729186721, 0.01472304088500942833, 0.01542409431272698944, 0.01612514774044455229, 0.01682620116816211167 ),
 .UNSPECIFIED. ) ;
#2636 = CARTESIAN_POINT ( 'NONE',  ( 14.20053099622510118, 1.593282007777887976, 35.07724096963458749 ) ) ;
#2637 = ORIENTED_EDGE ( 'NONE', *, *, #3023, .F. ) ;
#2638 = ORIENTED_EDGE ( 'NONE', *, *, #505, .T. ) ;
#2639 = APPLICATION_PROTOCOL_DEFINITION ( 'draft international standard', 'automotive_design', 1998, #2779 ) ;
#2640 = DIRECTION ( 'NONE',  ( 1.707404996040164265E-16, -1.000000000000000000, -0.000000000000000000 ) ) ;
#2641 = AXIS2_PLACEMENT_3D ( 'NONE', #1594, #2243, #3330 ) ;
#2642 = VERTEX_POINT ( 'NONE', #4109 ) ;
#2643 = VECTOR ( 'NONE', #112, 1000.000000000000000 ) ;
#2644 = CARTESIAN_POINT ( 'NONE',  ( 12.37117936981252342, 7.151597986548670960, 17.79394892777614601 ) ) ;
#2645 = CARTESIAN_POINT ( 'NONE',  ( 12.37117936981252164, -7.143402013451326305, 31.86762445358908735 ) ) ;
#2646 = LINE ( 'NONE', #106, #2031 ) ;
#2647 = CARTESIAN_POINT ( 'NONE',  ( -14.20057006193529858, 1.592637804043315564, 35.07746567129901649 ) ) ;
#2648 = DIRECTION ( 'NONE',  ( -0.000000000000000000, -0.000000000000000000, -1.000000000000000000 ) ) ;
#2649 = VECTOR ( 'NONE', #266, 1000.000000000000000 ) ;
#2650 = EDGE_LOOP ( 'NONE', ( #3162, #4460, #3342, #2655 ) ) ;
#2651 = DIRECTION ( 'NONE',  ( 0.000000000000000000, -1.000000000000000000, 0.000000000000000000 ) ) ;
#2652 = FACE_OUTER_BOUND ( 'NONE', #211, .T. ) ;
#2653 = CARTESIAN_POINT ( 'NONE',  ( -17.48249276543803532, -7.893402013451320975, 17.90262445358908039 ) ) ;
#2654 = VECTOR ( 'NONE', #4066, 1000.000000000000000 ) ;
#2655 = ORIENTED_EDGE ( 'NONE', *, *, #961, .F. ) ;
#2656 = CARTESIAN_POINT ( 'NONE',  ( 18.74250723456195189, 3.577847986548670534, 31.86762445358909446 ) ) ;
#2657 = DIRECTION ( 'NONE',  ( -0.000000000000000000, -0.000000000000000000, -1.000000000000000000 ) ) ;
#2658 = CARTESIAN_POINT ( 'NONE',  ( -3.750000000000000888, -3.750000000000000000, 3.749999999999995559 ) ) ;
#2659 = EDGE_CURVE ( 'NONE', #2437, #1942, #578, .T. ) ;
#2660 = EDGE_LOOP ( 'NONE', ( #3577, #4016, #1959, #3829 ) ) ;
#2661 = ORIENTED_EDGE ( 'NONE', *, *, #3944, .F. ) ;
#2662 = ITEM_DEFINED_TRANSFORMATION ( 'NONE', 'NONE', #946,  #4483 ) ;
#2663 = LINE ( 'NONE', #4053, #1063 ) ;
#2664 = ORIENTED_EDGE ( 'NONE', *, *, #1666, .F. ) ;
#2665 = CARTESIAN_POINT ( 'NONE',  ( 4.762507234561953240, 0.004097986548672528061, -10.04237554641092345 ) ) ;
#2666 = CARTESIAN_POINT ( 'NONE',  ( 13.30105870961065584, 5.219633490845899892, 37.25417504454090079 ) ) ;
#2667 = CARTESIAN_POINT ( 'NONE',  ( 3.040000505521795571, -17.78000000000000114, 17.78000050552179445 ) ) ;
#2668 = DIRECTION ( 'NONE',  ( -1.000000000000000000, -1.076498916035107621E-16, 0.000000000000000000 ) ) ;
#2669 = VERTEX_POINT ( 'NONE', #2695 ) ;
#2670 = DIRECTION ( 'NONE',  ( 0.000000000000000000, -1.000000000000000000, 0.000000000000000000 ) ) ;
#2671 = ADVANCED_FACE ( 'NONE', ( #4466 ), #935, .T. ) ;
#2672 = CARTESIAN_POINT ( 'NONE',  ( 14.03228452734540177, 2.697812684413582573, 29.50746059750024486 ) ) ;
#2673 = CIRCLE ( 'NONE', #4333, 1.499999999999999556 ) ;
#2674 = ORIENTED_EDGE ( 'NONE', *, *, #57, .F. ) ;
#2675 = LINE ( 'NONE', #1151, #1043 ) ;
#2676 = EDGE_CURVE ( 'NONE', #1332, #116, #1790, .T. ) ;
#2677 = PRODUCT_DEFINITION_CONTEXT ( 'detailed design', #474, 'design' ) ;
#2678 = EDGE_CURVE ( 'NONE', #1846, #245, #3756, .T. ) ;
#2679 = CARTESIAN_POINT ( 'NONE',  ( 14.28750723456195537, 0.004097986548674278397, 28.29387445358909403 ) ) ;
#2680 = ADVANCED_BREP_SHAPE_REPRESENTATION ( '', ( #363, #4483 ), #4021 ) ;
#2681 = DIRECTION ( 'NONE',  ( 0.000000000000000000, 0.000000000000000000, -1.000000000000000000 ) ) ;
#2682 = EDGE_LOOP ( 'NONE', ( #1196, #1094, #658, #4282 ) ) ;
#2683 = ORIENTED_EDGE ( 'NONE', *, *, #4573, .T. ) ;
#2684 = ITEM_DEFINED_TRANSFORMATION ( 'NONE', 'NONE', #1331,  #4483 ) ;
#2685 = CARTESIAN_POINT ( 'NONE',  ( 3.040000505521796015, -3.039999999999999591, 17.28000050552179445 ) ) ;
#2686 = CARTESIAN_POINT ( 'NONE',  ( -9.549434556529077899E-17, 3.750000000000000000, 18.74999999999999645 ) ) ;
#2687 = UNCERTAINTY_MEASURE_WITH_UNIT (LENGTH_MEASURE( 1.000000000000000082E-05 ), #3953, 'distance_accuracy_value', 'NONE');
#2688 = VERTEX_POINT ( 'NONE', #3409 ) ;
#2689 = FACE_OUTER_BOUND ( 'NONE', #3208, .T. ) ;
#2690 = AXIS2_PLACEMENT_3D ( 'NONE', #2491, #708, #3934 ) ;
#2691 = CARTESIAN_POINT ( 'NONE',  ( 6.870005009003979701, -6.397499167952786614, 17.65096039353565160 ) ) ;
#2692 = CARTESIAN_POINT ( 'NONE',  ( -8.369992765438043492, 6.401597986548673624, 31.86762445358908735 ) ) ;
#2693 = CARTESIAN_POINT ( 'NONE',  ( 3.750000000000000000, 3.750000000000000000, 146.2500000000000000 ) ) ;
#2694 = DIRECTION ( 'NONE',  ( -1.000000000000000000, 0.000000000000000000, 0.000000000000000000 ) ) ;
#2695 = CARTESIAN_POINT ( 'NONE',  ( 12.37117714425454551, 7.147500832047209762, 32.36596039353565857 ) ) ;
#2696 = B_SPLINE_CURVE_WITH_KNOTS ( 'NONE', 3,
 ( #3028, #1912, #4472, #2296, #1213, #2956, #117, #4425, #516, #3738, #1190, #3343, #3691, #473, #1839, #2926, #4376, #1110 ),
 .UNSPECIFIED., .F., .F.,
 ( 4, 2, 2, 2, 2, 2, 2, 2, 4 ),
 ( 0.000000000000000000, 0.0007012932024186013802, 0.001402586404837202760, 0.002103879607255804141, 0.002805172809674405521, 0.003506466012093006901, 0.004207759214511608281, 0.004909052416930209661, 0.005610345619348811042 ),
 .UNSPECIFIED. ) ;
#2697 = EDGE_LOOP ( 'NONE', ( #3840, #402, #2078, #1178, #2987 ) ) ;
#2698 = CIRCLE ( 'NONE', #2620, 4.762499999999999289 ) ;
#2699 = CARTESIAN_POINT ( 'NONE',  ( -8.369992765438045268, -6.393402013451322752, 3.292624453589076960 ) ) ;
#2700 = DIRECTION ( 'NONE',  ( 0.000000000000000000, 0.000000000000000000, -1.000000000000000000 ) ) ;
#2701 = EDGE_CURVE ( 'NONE', #2006, #4636, #447, .T. ) ;
#2702 = EDGE_LOOP ( 'NONE', ( #2034, #3530, #1123, #842, #584 ) ) ;
#2703 = DIRECTION ( 'NONE',  ( 1.000000000000000000, 0.000000000000000000, 0.000000000000000000 ) ) ;
#2704 = DIRECTION ( 'NONE',  ( 1.000000000000000000, 0.000000000000000000, 0.000000000000000000 ) ) ;
#2705 = ORIENTED_EDGE ( 'NONE', *, *, #113, .F. ) ;
#2706 = VECTOR ( 'NONE', #2271, 1000.000000000000000 ) ;
#2707 = EDGE_LOOP ( 'NONE', ( #2323, #2392, #3078, #2937, #3977 ) ) ;
#2708 = CARTESIAN_POINT ( 'NONE',  ( -12.37116712624658810, -7.147499167952783061, 32.36596039353565857 ) ) ;
#2709 = DIRECTION ( 'NONE',  ( 1.000000000000000000, -0.000000000000000000, -0.000000000000000000 ) ) ;
#2710 = VECTOR ( 'NONE', #3920, 1000.000000000000000 ) ;
#2711 = ORIENTED_EDGE ( 'NONE', *, *, #846, .T. ) ;
#2712 = CYLINDRICAL_SURFACE ( 'NONE', #2599, 0.5000000000000004441 ) ;
#2713 = CARTESIAN_POINT ( 'NONE',  ( 6.586250505521797471, -10.16000000000000014, 6.586250505521798360 ) ) ;
#2714 = CARTESIAN_POINT ( 'NONE',  ( 10.62689197487892478, 3.330708927240794814, 56.18096039353566340 ) ) ;
#2715 = DIRECTION ( 'NONE',  ( -1.000000000000000000, 1.076498916035107744E-16, 0.000000000000000000 ) ) ;
#2716 = CARTESIAN_POINT ( 'NONE',  ( 14.09723262389519149, 2.335210255262312184, 39.12537387803049427 ) ) ;
#2717 = DIRECTION ( 'NONE',  ( -0.000000000000000000, -0.000000000000000000, -1.000000000000000000 ) ) ;
#2718 = CARTESIAN_POINT ( 'NONE',  ( -13.87970196760993069, -3.386323001426799539, 30.71342844021988938 ) ) ;
#2719 = ORIENTED_EDGE ( 'NONE', *, *, #39, .T. ) ;
#2720 = CARTESIAN_POINT ( 'NONE',  ( 7.620005009003978813, 3.573750832047212000, 32.36596039353566567 ) ) ;
#2721 = FACE_OUTER_BOUND ( 'NONE', #2526, .T. ) ;
#2722 =( REPRESENTATION_RELATIONSHIP ('NONE','NONE', #4401, #2171 ) REPRESENTATION_RELATIONSHIP_WITH_TRANSFORMATION ( #173 )SHAPE_REPRESENTATION_RELATIONSHIP( ) );
#2723 = ORIENTED_EDGE ( 'NONE', *, *, #3982, .T. ) ;
#2724 = DIRECTION ( 'NONE',  ( 0.000000000000000000, 0.000000000000000000, -1.000000000000000000 ) ) ;
#2725 = AXIS2_PLACEMENT_3D ( 'NONE', #3574, #3249, #24 ) ;
#2726 = CARTESIAN_POINT ( 'NONE',  ( 2.540000505521796015, -10.16000000000000014, 6.586250505521796583 ) ) ;
#2727 = EDGE_CURVE ( 'NONE', #4255, #4095, #3363, .T. ) ;
#2728 = VERTEX_POINT ( 'NONE', #4406 ) ;
#2729 = EDGE_LOOP ( 'NONE', ( #310, #3034, #4146, #1804 ) ) ;
#2730 = CARTESIAN_POINT ( 'NONE',  ( 13.73375050552179566, -8.066545718530848674, 6.586250505521797471 ) ) ;
#2731 = ORIENTED_EDGE ( 'NONE', *, *, #2128, .F. ) ;
#2732 = CARTESIAN_POINT ( 'NONE',  ( -17.48249276543803532, -7.143402013451320975, 3.292624453589076960 ) ) ;
#2733 = PRODUCT_DEFINITION_SHAPE ( 'NONE', 'NONE',  #4654 ) ;
#2734 = CARTESIAN_POINT ( 'NONE',  ( -18.58310853064287826, -6.829291578281000419, 46.02096039353565970 ) ) ;
#2735 = CARTESIAN_POINT ( 'NONE',  ( -12.50411890890981148, -6.913100685710334758, 34.24151272312386141 ) ) ;
#2736 = CARTESIAN_POINT ( 'NONE',  ( 12.39929143252201271, -7.099433306620209549, 33.31939447329314419 ) ) ;
#2737 = DIRECTION ( 'NONE',  ( 0.000000000000000000, 0.000000000000000000, 1.000000000000000000 ) ) ;
#2738 = DIRECTION ( 'NONE',  ( -0.000000000000000000, 0.000000000000000000, -1.000000000000000000 ) ) ;
#2739 = DIRECTION ( 'NONE',  ( 1.000000000000000000, 0.000000000000000000, 0.000000000000000000 ) ) ;
#2740 = DIRECTION ( 'NONE',  ( 1.076498916035107621E-16, -1.000000000000000000, 0.000000000000000000 ) ) ;
#2741 = ORIENTED_EDGE ( 'NONE', *, *, #4635, .F. ) ;
#2742 = AXIS2_PLACEMENT_3D ( 'NONE', #4202, #4610, #1416 ) ;
#2743 = PLANE ( 'NONE',  #283 ) ;
#2744 = EDGE_CURVE ( 'NONE', #3011, #1644, #2635, .T. ) ;
#2745 = PRODUCT_DEFINITION_SHAPE ( 'NONE', 'NONE',  #4652 ) ;
#2746 = DIRECTION ( 'NONE',  ( 1.000000000000000000, -0.000000000000000000, -0.000000000000000000 ) ) ;
#2747 = VERTEX_POINT ( 'NONE', #1194 ) ;
#2748 = ORIENTED_EDGE ( 'NONE', *, *, #773, .T. ) ;
#2749 = CIRCLE ( 'NONE', #3361, 0.5000000000000004441 ) ;
#2750 = CARTESIAN_POINT ( 'NONE',  ( 2.540000505521796015, -3.039999999999999147, 3.040000505521795571 ) ) ;
#2751 = EDGE_CURVE ( 'NONE', #4494, #2212, #128, .T. ) ;
#2752 = EDGE_CURVE ( 'NONE', #3396, #2359, #2229, .T. ) ;
#2753 = ORIENTED_EDGE ( 'NONE', *, *, #51, .T. ) ;
#2754 = CARTESIAN_POINT ( 'NONE',  ( 3.749999999999999556, -3.750000000000000888, 3.749999999999995559 ) ) ;
#2755 = DIRECTION ( 'NONE',  ( -0.7638180911518758220, -1.821459649775647141E-17, -0.6454315793553214720 ) ) ;
#2756 = CARTESIAN_POINT ( 'NONE',  ( -13.66281077095347207, -4.183336980462362575, 38.16598501014195932 ) ) ;
#2757 = CIRCLE ( 'NONE', #2530, 0.5000000000000004441 ) ;
#2758 = FACE_OUTER_BOUND ( 'NONE', #2660, .T. ) ;
#2759 = DIRECTION ( 'NONE',  ( -1.000000000000000000, 1.076498916035107744E-16, 0.000000000000000000 ) ) ;
#2760 = AXIS2_PLACEMENT_3D ( 'NONE', #4473, #2008, #3442 ) ;
#2761 = PLANE ( 'NONE',  #3616 ) ;
#2762 = CYLINDRICAL_SURFACE ( 'NONE', #1931, 3.573750000000000426 ) ;
#2763 = ORIENTED_EDGE ( 'NONE', *, *, #401, .F. ) ;
#2764 = LINE ( 'NONE', #1327, #468 ) ;
#2765 = DIRECTION ( 'NONE',  ( 1.000000000000000000, -1.076498916035107621E-16, 0.000000000000000000 ) ) ;
#2766 = ORIENTED_EDGE ( 'NONE', *, *, #3033, .T. ) ;
#2767 = LINE ( 'NONE', #631, #2906 ) ;
#2768 = VECTOR ( 'NONE', #821, 1000.000000000000000 ) ;
#2769 = LINE ( 'NONE', #3790, #1865 ) ;
#2770 = VERTEX_POINT ( 'NONE', #521 ) ;
#2771 = EDGE_LOOP ( 'NONE', ( #4181, #494, #630, #701 ) ) ;
#2772 = AXIS2_PLACEMENT_3D ( 'NONE', #2178, #2573, #3218 ) ;
#2773 = VECTOR ( 'NONE', #276, 1000.000000000000000 ) ;
#2774 = VERTEX_POINT ( 'NONE', #1965 ) ;
#2775 = FACE_OUTER_BOUND ( 'NONE', #4165, .T. ) ;
#2776 = DIRECTION ( 'NONE',  ( -1.000000000000000000, 1.076498916035107744E-16, 0.000000000000000000 ) ) ;
#2777 = EDGE_CURVE ( 'NONE', #1450, #1649, #3394, .T. ) ;
#2778 = B_SPLINE_CURVE_WITH_KNOTS ( 'NONE', 3,
 ( #3240, #1902, #2879, #414, #2524, #1534, #3967, #1553, #1881, #1509, #3660, #2971, #4323, #1108, #2248, #2924, #739, #1134 ),
 .UNSPECIFIED., .F., .F.,
 ( 4, 2, 2, 2, 2, 2, 2, 2, 4 ),
 ( 0.01682620116816211167, 0.01752698813223788760, 0.01822777509631366005, 0.01892856206038943251, 0.01962934902446520843, 0.02033013598854098089, 0.02103092295261675682, 0.02173170991669252927, 0.02243249688076830173 ),
 .UNSPECIFIED. ) ;
#2779 = APPLICATION_CONTEXT ( 'automotive_design' ) ;
#2780 = B_SPLINE_CURVE_WITH_KNOTS ( 'NONE', 3,
 ( #2030, #169, #1499, #1529, #4117, #4387, #2590, #4028, #803, #3739, #517, #1961, #544, #3417, #191, #4590, #1724, #2412 ),
 .UNSPECIFIED., .F., .F.,
 ( 4, 2, 2, 2, 2, 2, 2, 2, 4 ),
 ( 1.014071938996880503E-18, 0.0007013035162779028249, 0.001402607032555804783, 0.002103910548833706415, 0.002805214065111607830, 0.003506517581389509246, 0.004207821097667410228, 0.004909124613945311209, 0.005610428130223212191 ),
 .UNSPECIFIED. ) ;
#2781 = CARTESIAN_POINT ( 'NONE',  ( 14.28750500900398279, 8.320472145597748469E-07, 3.790960393535649064 ) ) ;
#2782 = CARTESIAN_POINT ( 'NONE',  ( -6.869994990996021400, -6.397499167952784838, 17.65096039353565160 ) ) ;
#2783 =( NAMED_UNIT ( * ) SI_UNIT ( $, .STERADIAN. ) SOLID_ANGLE_UNIT ( ) );
#2784 = MECHANICAL_DESIGN_GEOMETRIC_PRESENTATION_REPRESENTATION (  '', ( #540 ), #2561 ) ;
#2785 = ADVANCED_FACE ( 'NONE', ( #1642 ), #1986, .F. ) ;
#2786 = CARTESIAN_POINT ( 'NONE',  ( -14.26312048591866599, -0.9355300642538868505, 28.38824789321300912 ) ) ;
#2787 = LINE ( 'NONE', #1396, #3965 ) ;
#2788 = FACE_OUTER_BOUND ( 'NONE', #4647, .T. ) ;
#2789 = DIRECTION ( 'NONE',  ( -0.000000000000000000, 1.000000000000000000, -0.000000000000000000 ) ) ;
#2790 = ORIENTED_EDGE ( 'NONE', *, *, #3155, .F. ) ;
#2791 = CARTESIAN_POINT ( 'NONE',  ( 7.234561953626996335E-06, 0.004097986548672528061, 3.292624453589077405 ) ) ;
#2792 = FACE_OUTER_BOUND ( 'NONE', #2079, .T. ) ;
#2793 = VERTEX_POINT ( 'NONE', #3670 ) ;
#2794 = AXIS2_PLACEMENT_3D ( 'NONE', #220, #949, #1291 ) ;
#2795 = ORIENTED_EDGE ( 'NONE', *, *, #2887, .F. ) ;
#2796 = SHAPE_REPRESENTATION ( 'Part 136_Varsay\X2\0131\X0\lan', ( #4483 ), #4552 ) ;
#2797 = EDGE_CURVE ( 'NONE', #3571, #1713, #2749, .T. ) ;
#2798 = CARTESIAN_POINT ( 'NONE',  ( -8.369992765438045268, -6.393402013451324528, 17.90262445358908039 ) ) ;
#2799 = AXIS2_PLACEMENT_3D ( 'NONE', #3587, #1128, #1053 ) ;
#2800 = ORIENTED_EDGE ( 'NONE', *, *, #183, .T. ) ;
#2801 = CARTESIAN_POINT ( 'NONE',  ( 12.13220478356813636, 7.546708218815218139, 17.73167833386938597 ) ) ;
#2802 = ORIENTED_EDGE ( 'NONE', *, *, #2552, .F. ) ;
#2803 = CARTESIAN_POINT ( 'NONE',  ( 3.040000505521795571, -17.28000000000000114, 17.28000050552179445 ) ) ;
#2804 = DIRECTION ( 'NONE',  ( 1.000000000000000000, 3.514501480744010632E-17, 1.502974711462165309E-16 ) ) ;
#2805 = DIRECTION ( 'NONE',  ( 1.000000000000000000, 1.076498916035107621E-16, -0.000000000000000000 ) ) ;
#2806 = DIRECTION ( 'NONE',  ( 1.000000000000000000, 0.000000000000000000, 0.000000000000000000 ) ) ;
#2807 = CARTESIAN_POINT ( 'NONE',  ( 18.74250723456195189, 3.577847986548670534, 31.86762445358909446 ) ) ;
#2808 = CYLINDRICAL_SURFACE ( 'NONE', #1392, 0.7499999999999997780 ) ;
#2809 = CARTESIAN_POINT ( 'NONE',  ( 13.83333314027810523, -3.573749167952788408, 32.36596039353566567 ) ) ;
#2810 = LINE ( 'NONE', #1702, #3950 ) ;
#2811 = LINE ( 'NONE', #3896, #3324 ) ;
#2812 = DIRECTION ( 'NONE',  ( -1.000000000000000000, -0.000000000000000000, -0.000000000000000000 ) ) ;
#2813 = VERTEX_POINT ( 'NONE', #2726 ) ;
#2814 = ADVANCED_FACE ( 'NONE', ( #3156 ), #990, .T. ) ;
#2815 = CARTESIAN_POINT ( 'NONE',  ( 12.62992896695153178, -6.676319002079077691, 34.41960495102417639 ) ) ;
#2816 =( GEOMETRIC_REPRESENTATION_CONTEXT ( 3 ) GLOBAL_UNCERTAINTY_ASSIGNED_CONTEXT ( ( #1622 ) ) GLOBAL_UNIT_ASSIGNED_CONTEXT ( ( #4035, #859, #458 ) ) REPRESENTATION_CONTEXT ( 'NONE', 'WORKASPACE' ) );
#2817 = LINE ( 'NONE', #1039, #2654 ) ;
#2818 = CIRCLE ( 'NONE', #4633, 3.573749999999998650 ) ;
#2819 = ORIENTED_EDGE ( 'NONE', *, *, #123, .F. ) ;
#2820 = ORIENTED_EDGE ( 'NONE', *, *, #2531, .T. ) ;
#2821 = EDGE_CURVE ( 'NONE', #4620, #1168, #1380, .T. ) ;
#2822 =( BOUNDED_CURVE ( )  B_SPLINE_CURVE ( 3, ( #1565, #2982, #1214, #2631 ),
 .UNSPECIFIED., .F., .T. ) 
 B_SPLINE_CURVE_WITH_KNOTS ( ( 4, 4 ),
 ( 4.712388980384689674, 6.283185307179586232 ),
 .UNSPECIFIED. ) 
 CURVE ( )  GEOMETRIC_REPRESENTATION_ITEM ( )  RATIONAL_B_SPLINE_CURVE ( ( 1.000000000000000000, 0.8047378541243649375, 0.8047378541243649375, 1.000000000000000000 ) ) 
 REPRESENTATION_ITEM ( '' )  );
#2823 = CARTESIAN_POINT ( 'NONE',  ( -13.83077811249668976, 3.610099873504223122, 38.05628366828691611 ) ) ;
#2824 = AXIS2_PLACEMENT_3D ( 'NONE', #1960, #3389, #820 ) ;
#2825 = PRODUCT ( 'Part 130_Varsay\X2\0131\X0\lan', 'Part 130_Varsay\X2\0131\X0\lan', '', ( #1075 ) ) ;
#2826 = EDGE_LOOP ( 'NONE', ( #417, #50, #1531, #4217, #53, #396, #2167, #1084, #2056, #3762, #511, #4629 ) ) ;
#2827 = CARTESIAN_POINT ( 'NONE',  ( 17.28000050552179445, -2.539999999999996927, 17.28000050552179445 ) ) ;
#2828 = VERTEX_POINT ( 'NONE', #565 ) ;
#2829 = DIRECTION ( 'NONE',  ( -1.000000000000000000, 0.000000000000000000, 0.000000000000000000 ) ) ;
#2830 = CARTESIAN_POINT ( 'NONE',  ( -8.423108025121075926, 5.316958927240794885, -113.4690396064643636 ) ) ;
#2831 = CARTESIAN_POINT ( 'NONE',  ( 13.83943268946890193, -3.550368327121672163, 31.89570794180626123 ) ) ;
#2832 = DIRECTION ( 'NONE',  ( 1.076498916035107744E-16, 1.000000000000000000, 0.000000000000000000 ) ) ;
#2833 = CARTESIAN_POINT ( 'NONE',  ( -3.152215195724335839, -3.565902013451327068, -1.469875546410923661 ) ) ;
#2834 = DIRECTION ( 'NONE',  ( 1.000000000000000000, 0.000000000000000000, 0.000000000000000000 ) ) ;
#2835 = CIRCLE ( 'NONE', #1425, 7.147499999999999076 ) ;
#2836 = DIRECTION ( 'NONE',  ( -1.000000000000000000, -8.673617379884035472E-17, 0.000000000000000000 ) ) ;
#2837 = CARTESIAN_POINT ( 'NONE',  ( 7.620007234561951392, 6.401597986548672736, 17.15262445358908039 ) ) ;
#2838 = ORIENTED_EDGE ( 'NONE', *, *, #1582, .T. ) ;
#2839 = CARTESIAN_POINT ( 'NONE',  ( 17.28000050552179800, -17.28000000000000114, 17.28000050552179445 ) ) ;
#2840 = EDGE_CURVE ( 'NONE', #2642, #4262, #4166, .T. ) ;
#2841 = CARTESIAN_POINT ( 'NONE',  ( -17.48249276543803532, -7.893402013451320975, 17.90262445358908039 ) ) ;
#2842 = ORIENTED_EDGE ( 'NONE', *, *, #20, .T. ) ;
#2843 = ORIENTED_EDGE ( 'NONE', *, *, #265, .T. ) ;
#2844 = CARTESIAN_POINT ( 'NONE',  ( -14.26330168061722148, 0.9562767277516133202, 38.96710911585693538 ) ) ;
#2845 = VERTEX_POINT ( 'NONE', #924 ) ;
#2846 = CARTESIAN_POINT ( 'NONE',  ( 14.99250500900398109, 7.897500832047208874, 18.40096039353565160 ) ) ;
#2847 = ORIENTED_EDGE ( 'NONE', *, *, #3740, .F. ) ;
#2848 = DIRECTION ( 'NONE',  ( 1.000000000000000000, -1.076498916035107621E-16, 0.000000000000000000 ) ) ;
#2849 = APPLICATION_PROTOCOL_DEFINITION ( 'draft international standard', 'automotive_design', 1998, #1115 ) ;
#2850 = CARTESIAN_POINT ( 'NONE',  ( 13.93158687739336088, 3.203336587929628720, 38.27608545593859901 ) ) ;
#2851 = AXIS2_PLACEMENT_3D ( 'NONE', #3290, #693, #2153 ) ;
#2852 = DIRECTION ( 'NONE',  ( -0.000000000000000000, 0.000000000000000000, -1.000000000000000000 ) ) ;
#2853 = CARTESIAN_POINT ( 'NONE',  ( -14.03269742075053195, 2.691508642874120394, 30.00328177004153574 ) ) ;
#2854 = DIRECTION ( 'NONE',  ( 1.000000000000000000, 0.000000000000000000, 0.000000000000000000 ) ) ;
#2855 = EDGE_CURVE ( 'NONE', #3260, #4527, #2055, .T. ) ;
#2856 = DIRECTION ( 'NONE',  ( -1.000000000000000000, 0.000000000000000000, 0.000000000000000000 ) ) ;
#2857 = VERTEX_POINT ( 'NONE', #4525 ) ;
#2858 = DIRECTION ( 'NONE',  ( 1.000000000000000000, 0.000000000000000000, 0.000000000000000000 ) ) ;
#2859 = VECTOR ( 'NONE', #4030, 1000.000000000000000 ) ;
#2860 = ADVANCED_FACE ( 'NONE', ( #656 ), #3812, .F. ) ;
#2861 = FACE_OUTER_BOUND ( 'NONE', #754, .T. ) ;
#2862 = CIRCLE ( 'NONE', #243, 0.7500000000000006661 ) ;
#2863 = ORIENTED_EDGE ( 'NONE', *, *, #2678, .F. ) ;
#2864 = EDGE_LOOP ( 'NONE', ( #2349, #4000, #3186 ) ) ;
#2865 = CARTESIAN_POINT ( 'NONE',  ( -14.10221755691438972, 2.339333233612962193, 38.63906452781715473 ) ) ;
#2866 = EDGE_CURVE ( 'NONE', #566, #2857, #2344, .T. ) ;
#2867 = VERTEX_POINT ( 'NONE', #3492 ) ;
#2868 = ORIENTED_EDGE ( 'NONE', *, *, #712, .T. ) ;
#2869 = LINE ( 'NONE', #4597, #3369 ) ;
#2870 = DIRECTION ( 'NONE',  ( 1.000000000000000000, 0.000000000000000000, 0.000000000000000000 ) ) ;
#2871 = CARTESIAN_POINT ( 'NONE',  ( -3.749994990996019517, 3.750000832047212906, 3.790960393535649064 ) ) ;
#2872 = DIRECTION ( 'NONE',  ( 1.000000000000000000, 0.000000000000000000, 0.000000000000000000 ) ) ;
#2873 = CIRCLE ( 'NONE', #2725, 3.573749999999999538 ) ;
#2874 = DIRECTION ( 'NONE',  ( -0.000000000000000000, -0.000000000000000000, -1.000000000000000000 ) ) ;
#2875 = CARTESIAN_POINT ( 'NONE',  ( -14.12120469946661494, -2.182301628983542852, 29.52629215715650091 ) ) ;
#2876 = CARTESIAN_POINT ( 'NONE',  ( 5.009003980371977336E-06, 3.750000832047212906, 18.79096039353565217 ) ) ;
#2877 = DIRECTION ( 'NONE',  ( -0.000000000000000000, -0.000000000000000000, -1.000000000000000000 ) ) ;
#2878 = FACE_BOUND ( 'NONE', #4444, .T. ) ;
#2879 = CARTESIAN_POINT ( 'NONE',  ( 14.28168262043153725, -0.4640750791195977776, 35.41829268623339289 ) ) ;
#2880 = SURFACE_STYLE_FILL_AREA ( #393 ) ;
#2881 = FACE_OUTER_BOUND ( 'NONE', #2650, .T. ) ;
#2882 = ORIENTED_EDGE ( 'NONE', *, *, #659, .T. ) ;
#2883 = DIRECTION ( 'NONE',  ( 0.000000000000000000, 1.000000000000000000, 0.000000000000000000 ) ) ;
#2884 = FACE_OUTER_BOUND ( 'NONE', #2864, .T. ) ;
#2885 = ORIENTED_EDGE ( 'NONE', *, *, #2076, .T. ) ;
#2886 = ORIENTED_EDGE ( 'NONE', *, *, #2962, .T. ) ;
#2887 = EDGE_CURVE ( 'NONE', #4499, #3035, #3732, .T. ) ;
#2888 = LINE ( 'NONE', #3183, #4583 ) ;
#2889 = ORIENTED_EDGE ( 'NONE', *, *, #2329, .F. ) ;
#2890 = CARTESIAN_POINT ( 'NONE',  ( -13.83332089671217169, 3.577847986548673642, 31.86762445358909446 ) ) ;
#2891 =( GEOMETRIC_REPRESENTATION_CONTEXT ( 3 ) GLOBAL_UNCERTAINTY_ASSIGNED_CONTEXT ( ( #569 ) ) GLOBAL_UNIT_ASSIGNED_CONTEXT ( ( #2969, #504, #3776 ) ) REPRESENTATION_CONTEXT ( 'NONE', 'WORKASPACE' ) );
#2892 = DIRECTION ( 'NONE',  ( 1.000000000000000000, 1.665334536937734318E-16, 3.825249650243476815E-17 ) ) ;
#2893 = EDGE_CURVE ( 'NONE', #2006, #4494, #1268, .T. ) ;
#2894 = VECTOR ( 'NONE', #3994, 1000.000000000000000 ) ;
#2895 = EDGE_CURVE ( 'NONE', #421, #3489, #2769, .T. ) ;
#2896 = CARTESIAN_POINT ( 'NONE',  ( 0.2894426067789017121, -3.565902013451327512, -9.725952605682453012 ) ) ;
#2897 = ADVANCED_FACE ( 'NONE', ( #2792 ), #799, .T. ) ;
#2898 = CARTESIAN_POINT ( 'NONE',  ( -13.92247150553487600, 3.210277310620725633, 30.77820937948456503 ) ) ;
#2899 = CARTESIAN_POINT ( 'NONE',  ( 5.009003980371977336E-06, 8.320472128100606877E-07, 17.65096039353565160 ) ) ;
#2900 = EDGE_CURVE ( 'NONE', #2998, #1283, #4493, .T. ) ;
#2901 = CARTESIAN_POINT ( 'NONE',  ( 7.620005009003977037, 6.397500832047211539, 32.36596039353565857 ) ) ;
#2902 = CARTESIAN_POINT ( 'NONE',  ( 17.28000050552179800, -17.28000000000000114, 3.040000505521796015 ) ) ;
#2903 = EDGE_LOOP ( 'NONE', ( #3321, #2683, #3206, #1477 ) ) ;
#2904 = FACE_OUTER_BOUND ( 'NONE', #2826, .T. ) ;
#2905 = CARTESIAN_POINT ( 'NONE',  ( 13.73375050552179744, -10.16000000000000014, 2.540000505521796015 ) ) ;
#2906 = VECTOR ( 'NONE', #3900, 1000.000000000000000 ) ;
#2907 = CARTESIAN_POINT ( 'NONE',  ( 3.152229664848242852, -3.565902013451327068, -1.469875546410923661 ) ) ;
#2908 = VECTOR ( 'NONE', #5, 1000.000000000000000 ) ;
#2909 = ORIENTED_EDGE ( 'NONE', *, *, #4276, .F. ) ;
#2910 = VERTEX_POINT ( 'NONE', #1706 ) ;
#2911 = ORIENTED_EDGE ( 'NONE', *, *, #2797, .F. ) ;
#2912 = VECTOR ( 'NONE', #4606, 1000.000000000000000 ) ;
#2913 = EDGE_LOOP ( 'NONE', ( #1441, #3995 ) ) ;
#2914 = CARTESIAN_POINT ( 'NONE',  ( 7.234561953626996335E-06, 0.004097986548672528061, 3.292624453589077405 ) ) ;
#2915 = APPLICATION_PROTOCOL_DEFINITION ( 'draft international standard', 'automotive_design', 1998, #3119 ) ;
#2916 = CARTESIAN_POINT ( 'NONE',  ( 14.28750500900397746, 0.2341033329457500312, 28.79221039353566525 ) ) ;
#2917 = AXIS2_PLACEMENT_3D ( 'NONE', #1544, #4452, #4071 ) ;
#2918 = DIRECTION ( 'NONE',  ( -1.000000000000000000, 1.076498916035107621E-16, -0.000000000000000000 ) ) ;
#2919 = ADVANCED_FACE ( 'NONE', ( #261 ), #2602, .T. ) ;
#2920 = CARTESIAN_POINT ( 'NONE',  ( 7.234561953626996335E-06, 0.004097986548672528061, 17.15262445358908039 ) ) ;
#2921 = CYLINDRICAL_SURFACE ( 'NONE', #4178, 14.28750000000000142 ) ;
#2922 = FACE_OUTER_BOUND ( 'NONE', #4517, .T. ) ;
#2923 = CIRCLE ( 'NONE', #4362, 3.573749999999999538 ) ;
#2924 = CARTESIAN_POINT ( 'NONE',  ( 13.83942910803283688, -3.546298317252753574, 32.33825509850257873 ) ) ;
#2925 = DIRECTION ( 'NONE',  ( 1.000000000000000000, 0.000000000000000000, 0.000000000000000000 ) ) ;
#2926 = CARTESIAN_POINT ( 'NONE',  ( 14.28175077624798739, -0.4627368126066581655, 28.31667831377500377 ) ) ;
#2927 = EDGE_CURVE ( 'NONE', #3035, #338, #4639, .T. ) ;
#2928 = VECTOR ( 'NONE', #3570, 1000.000000000000000 ) ;
#2929 = ORIENTED_EDGE ( 'NONE', *, *, #4345, .T. ) ;
#2930 = CARTESIAN_POINT ( 'NONE',  ( 14.12152177866159874, 2.180236281663612719, 35.20712478225889441 ) ) ;
#2931 = CARTESIAN_POINT ( 'NONE',  ( -12.39925686550117945, -7.095362368031173261, 32.81963905935649706 ) ) ;
#2932 = VECTOR ( 'NONE', #1239, 1000.000000000000000 ) ;
#2933 = ORIENTED_EDGE ( 'NONE', *, *, #963, .F. ) ;
#2934 = CARTESIAN_POINT ( 'NONE',  ( -8.369994990996019624, -7.897499167952782173, 17.65096039353565160 ) ) ;
#2935 = DIRECTION ( 'NONE',  ( 1.000000000000000000, 0.000000000000000000, 0.000000000000000000 ) ) ;
#2936 = CARTESIAN_POINT ( 'NONE',  ( 3.040000505521796015, -17.28000000000000114, 3.040000505521796015 ) ) ;
#2937 = ORIENTED_EDGE ( 'NONE', *, *, #3937, .F. ) ;
#2938 = ORIENTED_EDGE ( 'NONE', *, *, #344, .T. ) ;
#2939 = DIRECTION ( 'NONE',  ( 0.000000000000000000, 0.000000000000000000, 1.000000000000000000 ) ) ;
#2940 = EDGE_CURVE ( 'NONE', #4575, #971, #552, .T. ) ;
#2941 = SHAPE_DEFINITION_REPRESENTATION ( #2118, #1005 ) ;
#2942 = CARTESIAN_POINT ( 'NONE',  ( 13.94776995008254694, -3.100015636283709242, 30.57263291037062203 ) ) ;
#2943 = ORIENTED_EDGE ( 'NONE', *, *, #4290, .T. ) ;
#2944 = FACE_BOUND ( 'NONE', #2460, .T. ) ;
#2945 = FACE_OUTER_BOUND ( 'NONE', #4027, .T. ) ;
#2946 = ADVANCED_FACE ( 'NONE', ( #1727 ), #4235, .T. ) ;
#2947 = FACE_OUTER_BOUND ( 'NONE', #635, .T. ) ;
#2948 = CARTESIAN_POINT ( 'NONE',  ( -13.86245741347044103, -3.455229889388735209, 32.79470164932398291 ) ) ;
#2949 = AXIS2_PLACEMENT_3D ( 'NONE', #1117, #3179, #1842 ) ;
#2950 = FACE_OUTER_BOUND ( 'NONE', #1572, .T. ) ;
#2951 = ORIENTED_EDGE ( 'NONE', *, *, #2450, .F. ) ;
#2952 = FACE_OUTER_BOUND ( 'NONE', #2490, .T. ) ;
#2953 = CARTESIAN_POINT ( 'NONE',  ( -14.09722038032925617, -2.331111436666425618, 38.62703793808391595 ) ) ;
#2954 = EDGE_CURVE ( 'NONE', #1408, #3035, #1667, .T. ) ;
#2955 = EDGE_LOOP ( 'NONE', ( #171, #4547, #77, #1358 ) ) ;
#2956 = CARTESIAN_POINT ( 'NONE',  ( 13.92256690490806115, -3.205812800917074767, 30.27923183374419125 ) ) ;
#2957 =( REPRESENTATION_RELATIONSHIP ('NONE','NONE', #4401, #2171 ) REPRESENTATION_RELATIONSHIP_WITH_TRANSFORMATION ( #2662 )SHAPE_REPRESENTATION_RELATIONSHIP( ) );
#2958 = CARTESIAN_POINT ( 'NONE',  ( -12.37116712624658099, 7.147500832047212427, 18.40096039353565160 ) ) ;
#2959 = EDGE_CURVE ( 'NONE', #4067, #3954, #3201, .T. ) ;
#2960 = CARTESIAN_POINT ( 'NONE',  ( 14.28155410871526065, 0.4758380746309069931, 35.41777643611839466 ) ) ;
#2961 = ORIENTED_EDGE ( 'NONE', *, *, #36, .F. ) ;
#2962 = EDGE_CURVE ( 'NONE', #3180, #3625, #2343, .T. ) ;
#2963 = ORIENTED_EDGE ( 'NONE', *, *, #1700, .F. ) ;
#2964 = DIRECTION ( 'NONE',  ( 1.000000000000000000, 1.076498916035107621E-16, -0.000000000000000000 ) ) ;
#2965 = CARTESIAN_POINT ( 'NONE',  ( -8.369992765438043492, 7.151597986548673624, 17.15262445358908039 ) ) ;
#2966 = VERTEX_POINT ( 'NONE', #2907 ) ;
#2967 = AXIS2_PLACEMENT_3D ( 'NONE', #1635, #38, #1483 ) ;
#2968 = FILL_AREA_STYLE_COLOUR ( '', #1528 ) ;
#2969 =( LENGTH_UNIT ( ) NAMED_UNIT ( * ) SI_UNIT ( .MILLI., .METRE. ) );
#2970 = CARTESIAN_POINT ( 'NONE',  ( -12.35745342653517653, 7.175449426168442280, 17.68815867240257589 ) ) ;
#2971 = CARTESIAN_POINT ( 'NONE',  ( 13.94778318531167471, -3.095894809702069761, 33.66111732484789343 ) ) ;
#2972 = DIRECTION ( 'NONE',  ( -0.000000000000000000, -0.000000000000000000, 1.000000000000000000 ) ) ;
#2973 = DIRECTION ( 'NONE',  ( 0.000000000000000000, 0.000000000000000000, 1.000000000000000000 ) ) ;
#2974 = AXIS2_PLACEMENT_3D ( 'NONE', #1183, #2181, #2249 ) ;
#2975 = VERTEX_POINT ( 'NONE', #333 ) ;
#2976 = DIRECTION ( 'NONE',  ( -1.000000000000000000, 1.076498916035107744E-16, 0.000000000000000000 ) ) ;
#2977 = CIRCLE ( 'NONE', #2369, 6.397499999999999964 ) ;
#2978 = CARTESIAN_POINT ( 'NONE',  ( 5.009003980371977336E-06, 8.320472128100606877E-07, 3.790960393535649064 ) ) ;
#2979 = DIRECTION ( 'NONE',  ( 0.000000000000000000, -1.000000000000000000, 0.000000000000000000 ) ) ;
#2980 = ORIENTED_EDGE ( 'NONE', *, *, #3586, .T. ) ;
#2981 = DIRECTION ( 'NONE',  ( -1.000000000000000000, 1.076498916035107744E-16, 0.000000000000000000 ) ) ;
#2982 = CARTESIAN_POINT ( 'NONE',  ( 12.25345478699094670, -13.73374999999999524, 8.066546224052645542 ) ) ;
#2983 = EDGE_CURVE ( 'NONE', #116, #1332, #2873, .T. ) ;
#2984 = AXIS2_PLACEMENT_3D ( 'NONE', #2384, #3490, #3531 ) ;
#2985 = DIRECTION ( 'NONE',  ( -1.000000000000000000, 1.076498916035107744E-16, -0.000000000000000000 ) ) ;
#2986 = ORIENTED_EDGE ( 'NONE', *, *, #185, .F. ) ;
#2987 = ORIENTED_EDGE ( 'NONE', *, *, #2206, .F. ) ;
#2988 = CARTESIAN_POINT ( 'NONE',  ( 14.09176629432668015, 2.362873823246649962, 29.67462178077400736 ) ) ;
#2989 = CARTESIAN_POINT ( 'NONE',  ( -13.83332312227014249, -3.573749167952786632, 32.36596039353566567 ) ) ;
#2990 = ORIENTED_EDGE ( 'NONE', *, *, #1516, .T. ) ;
#2991 = CARTESIAN_POINT ( 'NONE',  ( -12.37116712624657922, 7.147500832047210650, 32.84705871297352076 ) ) ;
#2992 = CARTESIAN_POINT ( 'NONE',  ( 13.73375050552179744, -10.16000000000000014, 13.73375050552179744 ) ) ;
#2993 =( LENGTH_UNIT ( ) NAMED_UNIT ( * ) SI_UNIT ( .MILLI., .METRE. ) );
#2994 = VECTOR ( 'NONE', #599, 1000.000000000000000 ) ;
#2995 = LINE ( 'NONE', #3334, #1435 ) ;
#2996 = CARTESIAN_POINT ( 'NONE',  ( 7.234561953626996335E-06, 0.004097986548672528061, 17.16762445358907385 ) ) ;
#2997 = DIRECTION ( 'NONE',  ( 0.000000000000000000, 0.000000000000000000, -1.000000000000000000 ) ) ;
#2998 = VERTEX_POINT ( 'NONE', #2119 ) ;
#2999 = ADVANCED_FACE ( 'NONE', ( #2884 ), #377, .T. ) ;
#3000 = DIRECTION ( 'NONE',  ( 0.000000000000000000, 0.000000000000000000, 1.000000000000000000 ) ) ;
#3001 = DIRECTION ( 'NONE',  ( -1.076498916035107621E-16, -1.000000000000000000, -8.841607930564763213E-17 ) ) ;
#3002 = ADVANCED_FACE ( 'NONE', ( #3901 ), #1445, .F. ) ;
#3003 = ORIENTED_EDGE ( 'NONE', *, *, #185, .T. ) ;
#3004 = CARTESIAN_POINT ( 'NONE',  ( -7.619994990996019624, -3.573749167952786188, 32.36596039353566567 ) ) ;
#3005 = EDGE_CURVE ( 'NONE', #4397, #1450, #3555, .T. ) ;
#3006 = PRODUCT_DEFINITION_CONTEXT ( 'detailed design', #4320, 'design' ) ;
#3007 = DIRECTION ( 'NONE',  ( -1.076498916035107621E-16, -1.000000000000000000, 0.000000000000000000 ) ) ;
#3008 = CIRCLE ( 'NONE', #3767, 3.573749999999999538 ) ;
#3009 = VECTOR ( 'NONE', #4087, 1000.000000000000000 ) ;
#3010 = ORIENTED_EDGE ( 'NONE', *, *, #2066, .T. ) ;
#3011 = VERTEX_POINT ( 'NONE', #1821 ) ;
#3012 = DIRECTION ( 'NONE',  ( -0.000000000000000000, -0.000000000000000000, -1.000000000000000000 ) ) ;
#3013 = CARTESIAN_POINT ( 'NONE',  ( -8.369994990996019624, -7.147499167952784838, 32.36596039353565857 ) ) ;
#3014 = ORIENTED_EDGE ( 'NONE', *, *, #3150, .F. ) ;
#3015 = ADVANCED_FACE ( 'NONE', ( #3974 ), #2459, .F. ) ;
#3016 = CARTESIAN_POINT ( 'NONE',  ( 17.78000050552179800, -17.28000000000000114, 3.040000505521795571 ) ) ;
#3017 = DIRECTION ( 'NONE',  ( -1.000000000000000000, 0.000000000000000000, -0.000000000000000000 ) ) ;
#3018 = CARTESIAN_POINT ( 'NONE',  ( -13.83332089671217524, 3.577847986548674086, 32.10183545663884530 ) ) ;
#3019 = CARTESIAN_POINT ( 'NONE',  ( 8.370005009003978813, 7.897500832047212427, 17.65096039353565160 ) ) ;
#3020 = ADVANCED_FACE ( 'NONE', ( #455 ), #2484, .F. ) ;
#3021 = COLOUR_RGB ( '', 0.66274510, 0.83137255, 0.94901961) ;
#3022 = ORIENTED_EDGE ( 'NONE', *, *, #3357, .T. ) ;
#3023 = EDGE_CURVE ( 'NONE', #4004, #3472, #178, .T. ) ;
#3024 = DIRECTION ( 'NONE',  ( -1.000000000000000000, 1.076498916035107744E-16, -0.000000000000000000 ) ) ;
#3025 = CARTESIAN_POINT ( 'NONE',  ( 13.83333536583607959, 3.577847986548671422, 31.63389550438917297 ) ) ;
#3026 = DIRECTION ( 'NONE',  ( 0.000000000000000000, -1.000000000000000000, 0.000000000000000000 ) ) ;
#3027 = ORIENTED_EDGE ( 'NONE', *, *, #1966, .F. ) ;
#3028 = CARTESIAN_POINT ( 'NONE',  ( 13.83333536583607781, -3.569652013451328543, 31.86762445358909446 ) ) ;
#3029 = CARTESIAN_POINT ( 'NONE',  ( 3.040000505521796015, -17.28000000000000114, 17.28000050552179445 ) ) ;
#3030 = LINE ( 'NONE', #1191, #4482 ) ;
#3031 = CARTESIAN_POINT ( 'NONE',  ( -7.619992765438045268, 3.577847986548672754, 31.86762445358909446 ) ) ;
#3032 = PRODUCT_DEFINITION_SHAPE ( 'NONE', 'NONE',  #4656 ) ;
#3033 = EDGE_CURVE ( 'NONE', #1779, #4527, #4615, .T. ) ;
#3034 = ORIENTED_EDGE ( 'NONE', *, *, #1934, .T. ) ;
#3035 = VERTEX_POINT ( 'NONE', #2210 ) ;
#3036 = CARTESIAN_POINT ( 'NONE',  ( 14.12133832020656676, 2.181416654277627654, 29.52570525180092176 ) ) ;
#3037 = DIRECTION ( 'NONE',  ( 0.000000000000000000, 0.000000000000000000, -1.000000000000000000 ) ) ;
#3038 = ORIENTED_EDGE ( 'NONE', *, *, #1858, .T. ) ;
#3039 = ADVANCED_FACE ( 'NONE', ( #700 ), #2139, .F. ) ;
#3040 = CARTESIAN_POINT ( 'NONE',  ( 12.35764476757788621, 7.175150426935585912, 17.68847735315404535 ) ) ;
#3041 = AXIS2_PLACEMENT_3D ( 'NONE', #3517, #1738, #2351 ) ;
#3042 = DIRECTION ( 'NONE',  ( 1.000000000000000000, -1.076498916035107621E-16, 0.000000000000000000 ) ) ;
#3043 = CARTESIAN_POINT ( 'NONE',  ( 13.73375050552179744, -10.16000000000000014, 13.73375050552179744 ) ) ;
#3044 = CARTESIAN_POINT ( 'NONE',  ( 6.870007234561952281, 6.401597986548672736, 17.15262445358908039 ) ) ;
#3045 = PLANE ( 'NONE',  #3055 ) ;
#3046 = CLOSED_SHELL ( 'NONE', ( #3700, #2400, #1962, #2242, #1209, #3736, #3854, #3375, #1492, #4542, #3512, #1732, #3395, #3049, #848, #3725, #1249, #328, #4152, #2035, #470, #769, #1537, #4223, #2410, #1447, #3002, #3176, #1137, #2946, #3114, #957, #2391, #4003, #485, #644, #3314, #944, #1641, #2919, #1938, #2168 ) ) ;
#3047 = AXIS2_PLACEMENT_3D ( 'NONE', #4299, #3307, #85 ) ;
#3048 = VERTEX_POINT ( 'NONE', #3223 ) ;
#3049 = ADVANCED_FACE ( 'NONE', ( #2861 ), #47, .T. ) ;
#3050 = FACE_OUTER_BOUND ( 'NONE', #2485, .T. ) ;
#3051 = EDGE_LOOP ( 'NONE', ( #2838, #3561, #2264, #1189, #1801 ) ) ;
#3052 = CARTESIAN_POINT ( 'NONE',  ( 2.540000505521796015, -17.78000000000000114, 17.78000050552179445 ) ) ;
#3053 = VECTOR ( 'NONE', #3668, 1000.000000000000000 ) ;
#3054 = ORIENTED_EDGE ( 'NONE', *, *, #2727, .T. ) ;
#3055 = AXIS2_PLACEMENT_3D ( 'NONE', #1228, #3073, #3729 ) ;
#3056 = LINE ( 'NONE', #3390, #3666 ) ;
#3057 = EDGE_CURVE ( 'NONE', #2613, #2486, #4389, .T. ) ;
#3058 = DIRECTION ( 'NONE',  ( 0.000000000000000000, 0.000000000000000000, -1.000000000000000000 ) ) ;
#3059 = VERTEX_POINT ( 'NONE', #1755 ) ;
#3060 = VERTEX_POINT ( 'NONE', #4616 ) ;
#3061 = CIRCLE ( 'NONE', #1038, 0.5000000000000004441 ) ;
#3062 = CARTESIAN_POINT ( 'NONE',  ( -14.10221978247235874, 2.335236079111500995, 39.13740046776371884 ) ) ;
#3063 = LINE ( 'NONE', #4193, #770 ) ;
#3064 = UNCERTAINTY_MEASURE_WITH_UNIT (LENGTH_MEASURE( 1.000000000000000082E-05 ), #3191, 'distance_accuracy_value', 'NONE');
#3065 = ORIENTED_EDGE ( 'NONE', *, *, #36, .T. ) ;
#3066 = CARTESIAN_POINT ( 'NONE',  ( 18.74250723456195189, 0.004097986548670510577, 31.86762445358909446 ) ) ;
#3067 = VECTOR ( 'NONE', #2017, 1000.000000000000000 ) ;
#3068 = CARTESIAN_POINT ( 'NONE',  ( 7.234561953626996335E-06, 0.004097986548672528061, -10.04237554641092345 ) ) ;
#3069 =( NAMED_UNIT ( * ) PLANE_ANGLE_UNIT ( ) SI_UNIT ( $, .RADIAN. ) );
#3070 = CARTESIAN_POINT ( 'NONE',  ( 10.16000050552179701, -10.16000000000000014, 17.78000050552179445 ) ) ;
#3071 = CARTESIAN_POINT ( 'NONE',  ( 13.93158465183538475, 3.199239433428168411, 38.77442139588518444 ) ) ;
#3072 = CARTESIAN_POINT ( 'NONE',  ( 7.234561953626996335E-06, 0.004097986548672528061, -10.04237554641092345 ) ) ;
#3073 = DIRECTION ( 'NONE',  ( -8.673617379884035472E-17, -1.000000000000000000, 0.000000000000000000 ) ) ;
#3074 = CARTESIAN_POINT ( 'NONE',  ( -14.09196505061983906, -2.357472998381126672, 29.17523161774379403 ) ) ;
#3075 = ORIENTED_EDGE ( 'NONE', *, *, #3866, .T. ) ;
#3076 = AXIS2_PLACEMENT_3D ( 'NONE', #1413, #959, #4535 ) ;
#3077 = CARTESIAN_POINT ( 'NONE',  ( -12.37116490068860664, 7.151597986548673624, 17.90262445358908039 ) ) ;
#3078 = ORIENTED_EDGE ( 'NONE', *, *, #3488, .T. ) ;
#3079 = CARTESIAN_POINT ( 'NONE',  ( 13.86273172203279991, 3.462389489571491730, 30.93651510420201234 ) ) ;
#3080 = EDGE_CURVE ( 'NONE', #1649, #4121, #2817, .T. ) ;
#3081 = ORIENTED_EDGE ( 'NONE', *, *, #2621, .F. ) ;
#3082 = CARTESIAN_POINT ( 'NONE',  ( 17.28000050552179445, -2.539999999999999591, 17.78000050552179445 ) ) ;
#3083 = CIRCLE ( 'NONE', #826, 14.28750000000000142 ) ;
#3084 = DIRECTION ( 'NONE',  ( -1.000000000000000000, 0.000000000000000000, 0.000000000000000000 ) ) ;
#3085 = EDGE_LOOP ( 'NONE', ( #73, #2417, #3926, #4236 ) ) ;
#3086 = ORIENTED_EDGE ( 'NONE', *, *, #3057, .T. ) ;
#3087 = CARTESIAN_POINT ( 'NONE',  ( 3.750000000000000888, -3.750000000000000000, 146.2500000000000000 ) ) ;
#3088 = AXIS2_PLACEMENT_3D ( 'NONE', #3072, #205, #3381 ) ;
#3089 = VECTOR ( 'NONE', #3288, 1000.000000000000000 ) ;
#3090 = ORIENTED_EDGE ( 'NONE', *, *, #2618, .F. ) ;
#3091 = CARTESIAN_POINT ( 'NONE',  ( 3.750000000000000888, -3.750000000000000000, 146.2500000000000000 ) ) ;
#3092 = VECTOR ( 'NONE', #2918, 1000.000000000000000 ) ;
#3093 = DIRECTION ( 'NONE',  ( 8.336371211934735792E-17, 1.000000000000000000, 0.000000000000000000 ) ) ;
#3094 = CARTESIAN_POINT ( 'NONE',  ( -14.00282433085553535, -2.840975162856891778, 34.54665773754472013 ) ) ;
#3095 = CARTESIAN_POINT ( 'NONE',  ( 12.25345478699094670, -13.73374999999999524, 12.25345478699094670 ) ) ;
#3096 = CARTESIAN_POINT ( 'NONE',  ( 3.040000505521796015, -2.539999999999999591, 17.28000050552179445 ) ) ;
#3097 = AXIS2_PLACEMENT_3D ( 'NONE', #2209, #3641, #420 ) ;
#3098 = ADVANCED_FACE ( 'NONE', ( #1234 ), #4233, .F. ) ;
#3099 = CARTESIAN_POINT ( 'NONE',  ( -14.28749499099602005, 8.320472128100571937E-07, 28.79221039353566880 ) ) ;
#3100 = ORIENTED_EDGE ( 'NONE', *, *, #4230, .F. ) ;
#3101 = DIRECTION ( 'NONE',  ( -1.000000000000000000, 0.000000000000000000, 0.000000000000000000 ) ) ;
#3102 = VERTEX_POINT ( 'NONE', #1608 ) ;
#3103 = DIRECTION ( 'NONE',  ( 8.673617379884035472E-17, -1.000000000000000000, 0.000000000000000000 ) ) ;
#3104 = CARTESIAN_POINT ( 'NONE',  ( -12.62991672338559468, 6.680417820674964702, 34.91794089097075471 ) ) ;
#3105 = ORIENTED_EDGE ( 'NONE', *, *, #3599, .T. ) ;
#3106 = DIRECTION ( 'NONE',  ( -0.000000000000000000, -0.000000000000000000, -1.000000000000000000 ) ) ;
#3107 = ADVANCED_FACE ( 'NONE', ( #3713 ), #3689, .T. ) ;
#3108 = ADVANCED_FACE ( 'NONE', ( #2231 ), #4400, .T. ) ;
#3109 = AXIS2_PLACEMENT_3D ( 'NONE', #1958, #2606, #3026 ) ;
#3110 = DIRECTION ( 'NONE',  ( -0.000000000000000000, -0.000000000000000000, -1.000000000000000000 ) ) ;
#3111 = EDGE_LOOP ( 'NONE', ( #1163, #3556, #282, #2731 ) ) ;
#3112 = EDGE_CURVE ( 'NONE', #3035, #2613, #793, .T. ) ;
#3113 = ORIENTED_EDGE ( 'NONE', *, *, #4114, .F. ) ;
#3114 = ADVANCED_FACE ( 'NONE', ( #4094 ), #471, .F. ) ;
#3115 = FACE_OUTER_BOUND ( 'NONE', #3421, .T. ) ;
#3116 = EDGE_CURVE ( 'NONE', #3620, #2845, #1086, .T. ) ;
#3117 = ORIENTED_EDGE ( 'NONE', *, *, #894, .T. ) ;
#3118 = CARTESIAN_POINT ( 'NONE',  ( 3.040000505521796015, -2.539999999999999591, 3.040000505521795571 ) ) ;
#3119 = APPLICATION_CONTEXT ( 'automotive_design' ) ;
#3120 = CARTESIAN_POINT ( 'NONE',  ( -14.28749499099602360, -0.2370289631965043498, 35.93971039353566965 ) ) ;
#3121 = CARTESIAN_POINT ( 'NONE',  ( 2.540000505521796015, -17.28000000000000114, 17.28000050552179445 ) ) ;
#3122 = CARTESIAN_POINT ( 'NONE',  ( -7.619992765438045268, -3.569652013451326322, 31.86762445358909446 ) ) ;
#3123 = CARTESIAN_POINT ( 'NONE',  ( 14.25924429792894088, -0.9271090578520909675, 35.82528087157432140 ) ) ;
#3124 = CARTESIAN_POINT ( 'NONE',  ( -3.750000000000000000, 3.750000000000000000, 3.749999999999995559 ) ) ;
#3125 = ORIENTED_EDGE ( 'NONE', *, *, #4281, .T. ) ;
#3126 = DIRECTION ( 'NONE',  ( -9.517981353260378315E-33, 8.841607930564763213E-17, -1.000000000000000000 ) ) ;
#3127 = AXIS2_PLACEMENT_3D ( 'NONE', #2492, #3262, #2870 ) ;
#3128 = ORIENTED_EDGE ( 'NONE', *, *, #4230, .T. ) ;
#3129 = AXIS2_PLACEMENT_3D ( 'NONE', #2899, #4342, #3289 ) ;
#3130 = CARTESIAN_POINT ( 'NONE',  ( 13.60369065225541974, -4.367129746283612945, 37.52732938813279873 ) ) ;
#3131 = CARTESIAN_POINT ( 'NONE',  ( 7.234561953626996335E-06, 0.004097986548672528061, -8.542375546410942988 ) ) ;
#3132 = ORIENTED_EDGE ( 'NONE', *, *, #996, .F. ) ;
#3133 = EDGE_LOOP ( 'NONE', ( #801, #222, #880, #94, #438 ) ) ;
#3134 = VECTOR ( 'NONE', #4503, 1000.000000000000000 ) ;
#3135 = SURFACE_STYLE_FILL_AREA ( #1711 ) ;
#3136 = ORIENTED_EDGE ( 'NONE', *, *, #2321, .T. ) ;
#3137 = DIRECTION ( 'NONE',  ( -1.076498916035107621E-16, -1.000000000000000000, 0.000000000000000000 ) ) ;
#3138 =( NAMED_UNIT ( * ) SI_UNIT ( $, .STERADIAN. ) SOLID_ANGLE_UNIT ( ) );
#3139 = CARTESIAN_POINT ( 'NONE',  ( -13.94746284641590428, -3.101372177908327199, 34.15706925759410950 ) ) ;
#3140 = VECTOR ( 'NONE', #2527, 1000.000000000000000 ) ;
#3141 = CARTESIAN_POINT ( 'NONE',  ( -8.369994990996016071, 6.397500832047212427, 3.790960393535649064 ) ) ;
#3142 = FACE_OUTER_BOUND ( 'NONE', #2279, .T. ) ;
#3143 = VECTOR ( 'NONE', #2776, 1000.000000000000000 ) ;
#3144 = PLANE ( 'NONE',  #311 ) ;
#3145 = DIRECTION ( 'NONE',  ( 1.000000000000000000, 0.000000000000000000, 0.000000000000000000 ) ) ;
#3146 = PLANE ( 'NONE',  #1964 ) ;
#3147 = CARTESIAN_POINT ( 'NONE',  ( -8.369992765438045268, 0.004097986548673428382, 31.86762445358908735 ) ) ;
#3148 = AXIS2_PLACEMENT_3D ( 'NONE', #4554, #2805, #1764 ) ;
#3149 = PRODUCT_RELATED_PRODUCT_CATEGORY ( 'part', '', ( #1031 ) ) ;
#3150 = EDGE_CURVE ( 'NONE', #3903, #1497, #1695, .T. ) ;
#3151 = ORIENTED_EDGE ( 'NONE', *, *, #4603, .T. ) ;
#3152 = EDGE_CURVE ( 'NONE', #2793, #3946, #3786, .T. ) ;
#3153 = CARTESIAN_POINT ( 'NONE',  ( -14.28749499099602005, 8.320472128100606877E-07, 17.65096039353565160 ) ) ;
#3154 = AXIS2_PLACEMENT_3D ( 'NONE', #2142, #3626, #3255 ) ;
#3155 = EDGE_CURVE ( 'NONE', #3954, #4040, #1471, .T. ) ;
#3156 = FACE_OUTER_BOUND ( 'NONE', #1863, .T. ) ;
#3157 = ORIENTED_EDGE ( 'NONE', *, *, #3500, .F. ) ;
#3158 = ORIENTED_EDGE ( 'NONE', *, *, #1875, .F. ) ;
#3159 = VECTOR ( 'NONE', #1373, 1000.000000000000000 ) ;
#3160 = SURFACE_STYLE_USAGE ( .BOTH. , #1731 ) ;
#3161 = VECTOR ( 'NONE', #88, 1000.000000000000000 ) ;
#3162 = ORIENTED_EDGE ( 'NONE', *, *, #3298, .T. ) ;
#3163 = LINE ( 'NONE', #2233, #3053 ) ;
#3164 = CARTESIAN_POINT ( 'NONE',  ( 10.16000050552179701, -13.73374999999999879, 10.16000050552179701 ) ) ;
#3165 = VECTOR ( 'NONE', #1566, 1000.000000000000000 ) ;
#3166 = PLANE ( 'NONE',  #3148 ) ;
#3167 = CARTESIAN_POINT ( 'NONE',  ( 8.370007234561949616, -6.393402013451325416, 17.90262445358908039 ) ) ;
#3168 = CARTESIAN_POINT ( 'NONE',  ( 8.370005009003978813, 6.397500832047211539, 32.36596039353565857 ) ) ;
#3169 = EDGE_CURVE ( 'NONE', #3326, #975, #2062, .T. ) ;
#3170 = FACE_OUTER_BOUND ( 'NONE', #2367, .T. ) ;
#3171 = PRODUCT_DEFINITION_SHAPE ( 'NONE', 'NONE',  #1640 ) ;
#3172 = DIRECTION ( 'NONE',  ( -1.000000000000000000, -0.000000000000000000, -0.000000000000000000 ) ) ;
#3173 = DIRECTION ( 'NONE',  ( 0.000000000000000000, 1.000000000000000000, -0.000000000000000000 ) ) ;
#3174 = FACE_OUTER_BOUND ( 'NONE', #477, .T. ) ;
#3175 = EDGE_CURVE ( 'NONE', #728, #2910, #3962, .T. ) ;
#3176 = ADVANCED_FACE ( 'NONE', ( #2544 ), #2808, .T. ) ;
#3177 = ORIENTED_EDGE ( 'NONE', *, *, #1103, .T. ) ;
#3178 = CARTESIAN_POINT ( 'NONE',  ( 14.10223202603829584, -2.331137260515613097, 38.63906452781715473 ) ) ;
#3179 = DIRECTION ( 'NONE',  ( 0.000000000000000000, 0.000000000000000000, 1.000000000000000000 ) ) ;
#3180 = VERTEX_POINT ( 'NONE', #3893 ) ;
#3181 = ORIENTED_EDGE ( 'NONE', *, *, #2584, .T. ) ;
#3182 = B_SPLINE_CURVE_WITH_KNOTS ( 'NONE', 3,
 ( #3099, #4536, #1325, #602, #3483, #2875, #1054, #1415, #3235, #3215, #322, #411, #4368, #691, #2200, #2218 ),
 .UNSPECIFIED., .F., .F.,
 ( 4, 2, 2, 2, 2, 2, 2, 4 ),
 ( 0.01121786453620354437, 0.01261999568898470973, 0.01332106126537529155, 0.01402212684176587336, 0.01472319241815645517, 0.01542425799454703872, 0.01612532357093762053, 0.01682638914732820234 ),
 .UNSPECIFIED. ) ;
#3183 = CARTESIAN_POINT ( 'NONE',  ( -3.750000000000000888, -3.750000000000000000, 18.74999999999999645 ) ) ;
#3184 = ORIENTED_EDGE ( 'NONE', *, *, #2983, .T. ) ;
#3185 = CARTESIAN_POINT ( 'NONE',  ( -8.369994990996016071, 6.397500832047212427, 32.36596039353565857 ) ) ;
#3186 = ORIENTED_EDGE ( 'NONE', *, *, #505, .F. ) ;
#3187 = CARTESIAN_POINT ( 'NONE',  ( -14.12139980767486946, 2.185052774741614190, 29.02700012481545144 ) ) ;
#3188 = DIRECTION ( 'NONE',  ( 1.110223024625156047E-16, -1.000000000000000000, 0.000000000000000000 ) ) ;
#3189 = CARTESIAN_POINT ( 'NONE',  ( -14.09151425697337778, -2.364203556260324302, 35.05593777286575374 ) ) ;
#3190 = CARTESIAN_POINT ( 'NONE',  ( 13.83333314027810523, -3.573749167952788408, 32.36596039353566567 ) ) ;
#3191 =( LENGTH_UNIT ( ) NAMED_UNIT ( * ) SI_UNIT ( .MILLI., .METRE. ) );
#3192 = DIRECTION ( 'NONE',  ( -9.517981353260378315E-33, -8.841607930564763213E-17, 1.000000000000000000 ) ) ;
#3193 = DIRECTION ( 'NONE',  ( -1.000000000000000000, 0.000000000000000000, 0.000000000000000000 ) ) ;
#3194 = EDGE_CURVE ( 'NONE', #1870, #2688, #4297, .T. ) ;
#3195 = CARTESIAN_POINT ( 'NONE',  ( 18.74250500900397753, -3.573749167952788852, 32.36596039353566567 ) ) ;
#3196 = DIRECTION ( 'NONE',  ( 1.000000000000000000, 0.000000000000000000, 0.000000000000000000 ) ) ;
#3197 = CARTESIAN_POINT ( 'NONE',  ( -3.749994990996019961, -3.749999167952787094, 17.65096039353565160 ) ) ;
#3198 = EDGE_LOOP ( 'NONE', ( #1609, #850 ) ) ;
#3199 = CARTESIAN_POINT ( 'NONE',  ( -12.37116712624658454, 7.147500832047209762, 18.40096039353565160 ) ) ;
#3200 = PRODUCT_DEFINITION_FORMATION_WITH_SPECIFIED_SOURCE ( 'ANY', '', #2403, .NOT_KNOWN. ) ;
#3201 = LINE ( 'NONE', #4280, #4009 ) ;
#3202 = AXIS2_PLACEMENT_3D ( 'NONE', #4273, #1081, #1055 ) ;
#3203 = ORIENTED_EDGE ( 'NONE', *, *, #1316, .F. ) ;
#3204 = ORIENTED_EDGE ( 'NONE', *, *, #166, .T. ) ;
#3205 = AXIS2_PLACEMENT_3D ( 'NONE', #4648, #1431, #3229 ) ;
#3206 = ORIENTED_EDGE ( 'NONE', *, *, #3857, .F. ) ;
#3207 = SPHERICAL_SURFACE ( 'NONE', #3205, 0.5000000000000000000 ) ;
#3208 = EDGE_LOOP ( 'NONE', ( #2322, #1361, #167, #1752, #889 ) ) ;
#3209 = PLANE ( 'NONE',  #2690 ) ;
#3210 = AXIS2_PLACEMENT_3D ( 'NONE', #109, #4234, #1011 ) ;
#3211 = APPLICATION_PROTOCOL_DEFINITION ( 'draft international standard', 'automotive_design', 1998, #474 ) ;
#3212 = CIRCLE ( 'NONE', #1195, 0.7499999999999997780 ) ;
#3213 = CARTESIAN_POINT ( 'NONE',  ( 14.17609192062688095, -1.791678206414217156, 29.26486561848145840 ) ) ;
#3214 = CARTESIAN_POINT ( 'NONE',  ( 17.28000050552179445, -3.039999999999999591, 3.040000505521795571 ) ) ;
#3215 = CARTESIAN_POINT ( 'NONE',  ( -13.94784893415634031, -3.099588501034327148, 30.57203322479964669 ) ) ;
#3216 = PLANE ( 'NONE',  #2514 ) ;
#3217 = VECTOR ( 'NONE', #3711, 1000.000000000000000 ) ;
#3218 = DIRECTION ( 'NONE',  ( -1.076498916035107621E-16, -1.000000000000000000, 0.000000000000000000 ) ) ;
#3219 = CARTESIAN_POINT ( 'NONE',  ( 17.78000050552179445, -10.16000000000000014, 10.16000050552179701 ) ) ;
#3220 = ORIENTED_EDGE ( 'NONE', *, *, #3740, .T. ) ;
#3221 = CARTESIAN_POINT ( 'NONE',  ( 14.25909138040731605, 0.9292885604723594151, 35.82465120474719811 ) ) ;
#3222 = EDGE_CURVE ( 'NONE', #4262, #3792, #1079, .T. ) ;
#3223 = CARTESIAN_POINT ( 'NONE',  ( 3.040000505521795571, -17.78000000000000114, 3.040000505521795571 ) ) ;
#3224 = ORIENTED_EDGE ( 'NONE', *, *, #1734, .T. ) ;
#3225 = VERTEX_POINT ( 'NONE', #735 ) ;
#3226 = VECTOR ( 'NONE', #1367, 1000.000000000000000 ) ;
#3227 = CARTESIAN_POINT ( 'NONE',  ( -13.60367618313151361, 4.375325719380958489, 37.52732938813279873 ) ) ;
#3228 = ORIENTED_EDGE ( 'NONE', *, *, #59, .T. ) ;
#3229 = DIRECTION ( 'NONE',  ( 1.000000000000000000, 0.000000000000000000, 0.000000000000000000 ) ) ;
#3230 = CARTESIAN_POINT ( 'NONE',  ( -14.09217321523874489, 2.364479724326565169, 29.17410210810483662 ) ) ;
#3231 = PRODUCT_CONTEXT ( 'NONE', #3358, 'mechanical' ) ;
#3232 = DIRECTION ( 'NONE',  ( -0.000000000000000000, -1.000000000000000000, -0.000000000000000000 ) ) ;
#3233 = CARTESIAN_POINT ( 'NONE',  ( 14.28174855069001303, -0.4668339671081180309, 28.81501425372158209 ) ) ;
#3234 = DIRECTION ( 'NONE',  ( -1.000000000000000000, 0.000000000000000000, 0.000000000000000000 ) ) ;
#3235 = CARTESIAN_POINT ( 'NONE',  ( -14.00274155455516478, -2.841332011922032663, 30.18594746002730744 ) ) ;
#3236 = FACE_OUTER_BOUND ( 'NONE', #3339, .T. ) ;
#3237 = FACE_OUTER_BOUND ( 'NONE', #2191, .T. ) ;
#3238 = DIRECTION ( 'NONE',  ( 0.000000000000000000, 0.000000000000000000, 1.000000000000000000 ) ) ;
#3239 = VECTOR ( 'NONE', #2497, 1000.000000000000000 ) ;
#3240 = CARTESIAN_POINT ( 'NONE',  ( 14.28750723456195537, 0.004097986548674313959, 35.44137445358909133 ) ) ;
#3241 = MECHANICAL_DESIGN_GEOMETRIC_PRESENTATION_REPRESENTATION (  '', ( #4292 ), #3315 ) ;
#3242 = CARTESIAN_POINT ( 'NONE',  ( 3.749999999999999556, -3.750000000000000888, 3.749999999999995559 ) ) ;
#3243 = CARTESIAN_POINT ( 'NONE',  ( 12.35746567010111185, -7.171350607572557045, 18.18649461234914710 ) ) ;
#3244 = EDGE_CURVE ( 'NONE', #4361, #3620, #3915, .T. ) ;
#3245 = ORIENTED_EDGE ( 'NONE', *, *, #995, .T. ) ;
#3246 = CARTESIAN_POINT ( 'NONE',  ( 10.16000050552179701, -6.586249999999999716, 10.16000050552179701 ) ) ;
#3247 = CIRCLE ( 'NONE', #2050, 0.5000000000000000000 ) ;
#3248 = CARTESIAN_POINT ( 'NONE',  ( -6.869992765438044380, 6.401597986548673624, 17.90262445358908039 ) ) ;
#3249 = DIRECTION ( 'NONE',  ( -1.000000000000000000, -1.076498916035107621E-16, 0.000000000000000000 ) ) ;
#3250 = AXIS2_PLACEMENT_3D ( 'NONE', #4042, #3665, #817 ) ;
#3251 = EDGE_CURVE ( 'NONE', #1657, #4, #3320, .T. ) ;
#3252 = VERTEX_POINT ( 'NONE', #2518 ) ;
#3253 = EDGE_CURVE ( 'NONE', #3887, #4134, #1481, .T. ) ;
#3254 = EDGE_LOOP ( 'NONE', ( #1378, #1089, #608, #593 ) ) ;
#3255 = DIRECTION ( 'NONE',  ( -1.000000000000000000, 0.000000000000000000, 0.000000000000000000 ) ) ;
#3256 = EDGE_CURVE ( 'NONE', #1617, #3903, #4144, .T. ) ;
#3257 = CIRCLE ( 'NONE', #3976, 14.28750000000000142 ) ;
#3258 = ORIENTED_EDGE ( 'NONE', *, *, #3112, .T. ) ;
#3259 = EDGE_CURVE ( 'NONE', #4620, #2910, #4607, .T. ) ;
#3260 = VERTEX_POINT ( 'NONE', #272 ) ;
#3261 = DIRECTION ( 'NONE',  ( -1.000000000000000000, 0.000000000000000000, 0.000000000000000000 ) ) ;
#3262 = DIRECTION ( 'NONE',  ( 0.000000000000000000, 0.000000000000000000, 1.000000000000000000 ) ) ;
#3263 = CARTESIAN_POINT ( 'NONE',  ( 12.50413115247574503, 6.917199504306219993, 33.74317678317729730 ) ) ;
#3264 = DIRECTION ( 'NONE',  ( 0.000000000000000000, 0.000000000000000000, 1.000000000000000000 ) ) ;
#3265 = CARTESIAN_POINT ( 'NONE',  ( 3.040000505521796015, -3.039999999999999147, 17.28000050552179445 ) ) ;
#3266 = CARTESIAN_POINT ( 'NONE',  ( -7.619992765438047044, -6.393402013451324528, 17.15262445358908039 ) ) ;
#3267 = CYLINDRICAL_SURFACE ( 'NONE', #2851, 0.7499999999999997780 ) ;
#3268 = FACE_OUTER_BOUND ( 'NONE', #2193, .T. ) ;
#3269 = CARTESIAN_POINT ( 'NONE',  ( -14.28749276543804925, 0.004097986548672528061, 17.15262445358908039 ) ) ;
#3270 = CARTESIAN_POINT ( 'NONE',  ( 12.27095706366207040, -7.318709742180212530, 17.91402383463540104 ) ) ;
#3271 = ORIENTED_EDGE ( 'NONE', *, *, #375, .T. ) ;
#3272 = DIRECTION ( 'NONE',  ( 1.000000000000000000, 0.000000000000000000, 0.000000000000000000 ) ) ;
#3273 = DIRECTION ( 'NONE',  ( -1.000000000000000000, 1.076498916035107744E-16, 0.000000000000000000 ) ) ;
#3274 = DIRECTION ( 'NONE',  ( -0.000000000000000000, -0.000000000000000000, -1.000000000000000000 ) ) ;
#3275 = EDGE_LOOP ( 'NONE', ( #4548, #1704, #3280, #4278, #684, #2029, #824, #1645 ) ) ;
#3276 = ORIENTED_EDGE ( 'NONE', *, *, #2135, .F. ) ;
#3277 =( LENGTH_UNIT ( ) NAMED_UNIT ( * ) SI_UNIT ( .MILLI., .METRE. ) );
#3278 = CLOSED_SHELL ( 'NONE', ( #3015, #2860, #4574, #4546, #2605, #1742, #4089, #1495, #1726, #2211, #3801, #3108, #2671, #2428, #1016, #4258, #925, #1454, #3595, #2258, #3874, #808, #3098, #4054, #1009, #2897, #1070, #3636, #3522, #1099, #1802, #2308, #4626, #1596, #2611, #4149 ) ) ;
#3279 = EDGE_CURVE ( 'NONE', #744, #4332, #384, .T. ) ;
#3280 = ORIENTED_EDGE ( 'NONE', *, *, #3284, .T. ) ;
#3281 = CARTESIAN_POINT ( 'NONE',  ( -14.17567385476558606, 1.798747337914841093, 28.76844003329341604 ) ) ;
#3282 = DIRECTION ( 'NONE',  ( -0.000000000000000000, -0.000000000000000000, -1.000000000000000000 ) ) ;
#3283 = VECTOR ( 'NONE', #1948, 1000.000000000000000 ) ;
#3284 = EDGE_CURVE ( 'NONE', #338, #4593, #2451, .T. ) ;
#3285 = CARTESIAN_POINT ( 'NONE',  ( 2.680752993293609165, -3.565902013451325736, -8.854438399834824835 ) ) ;
#3286 = AXIS2_PLACEMENT_3D ( 'NONE', #3131, #2077, #3084 ) ;
#3287 = FACE_OUTER_BOUND ( 'NONE', #2416, .T. ) ;
#3288 = DIRECTION ( 'NONE',  ( -1.000000000000000000, -0.000000000000000000, -0.000000000000000000 ) ) ;
#3289 = DIRECTION ( 'NONE',  ( -1.000000000000000000, 0.000000000000000000, 0.000000000000000000 ) ) ;
#3290 = CARTESIAN_POINT ( 'NONE',  ( 8.370005009003978813, 6.397500832047211539, 3.790960393535649064 ) ) ;
#3291 = DIRECTION ( 'NONE',  ( 1.000000000000000000, 0.000000000000000000, 0.000000000000000000 ) ) ;
#3292 = CARTESIAN_POINT ( 'NONE',  ( -9.549434556529077899E-17, -3.249382362871961689E-18, 131.2499999999999716 ) ) ;
#3293 = DIRECTION ( 'NONE',  ( -1.000000000000000000, 0.000000000000000000, 0.000000000000000000 ) ) ;
#3294 = ORIENTED_EDGE ( 'NONE', *, *, #2821, .T. ) ;
#3295 = CARTESIAN_POINT ( 'NONE',  ( 17.78000050552179445, -2.539999999999999591, 17.78000050552179445 ) ) ;
#3296 = DIRECTION ( 'NONE',  ( 9.517981353260378315E-33, -8.841607930564763213E-17, 1.000000000000000000 ) ) ;
#3297 = PRODUCT_DEFINITION ( 'UNKNOWN', '', #1707, #4474 ) ;
#3298 = EDGE_CURVE ( 'NONE', #2245, #1846, #2331, .T. ) ;
#3299 = VECTOR ( 'NONE', #619, 1000.000000000000000 ) ;
#3300 = ORIENTED_EDGE ( 'NONE', *, *, #3945, .T. ) ;
#3301 = FACE_OUTER_BOUND ( 'NONE', #3254, .T. ) ;
#3302 = ORIENTED_EDGE ( 'NONE', *, *, #286, .T. ) ;
#3303 = CIRCLE ( 'NONE', #1879, 0.7500000000000006661 ) ;
#3304 = ORIENTED_EDGE ( 'NONE', *, *, #2051, .T. ) ;
#3305 = DIRECTION ( 'NONE',  ( -1.000000000000000000, 0.000000000000000000, 0.000000000000000000 ) ) ;
#3306 = FACE_OUTER_BOUND ( 'NONE', #1399, .T. ) ;
#3307 = DIRECTION ( 'NONE',  ( -1.000000000000000000, 0.000000000000000000, 0.000000000000000000 ) ) ;
#3308 = DIRECTION ( 'NONE',  ( 1.000000000000000000, 0.000000000000000000, 0.000000000000000000 ) ) ;
#3309 = DIRECTION ( 'NONE',  ( 1.000000000000000000, 0.000000000000000000, 0.000000000000000000 ) ) ;
#3310 = AXIS2_PLACEMENT_3D ( 'NONE', #1515, #3296, #746 ) ;
#3311 = FACE_BOUND ( 'NONE', #355, .T. ) ;
#3312 = VERTEX_POINT ( 'NONE', #1745 ) ;
#3313 = CARTESIAN_POINT ( 'NONE',  ( 17.28000050552179445, -3.039999999999999591, 2.540000505521796015 ) ) ;
#3314 = ADVANCED_FACE ( 'NONE', ( #3170 ), #2761, .F. ) ;
#3315 =( GEOMETRIC_REPRESENTATION_CONTEXT ( 3 ) GLOBAL_UNCERTAINTY_ASSIGNED_CONTEXT ( ( #3064 ) ) GLOBAL_UNIT_ASSIGNED_CONTEXT ( ( #3191, #624, #2783 ) ) REPRESENTATION_CONTEXT ( 'NONE', 'WORKASPACE' ) );
#3316 = CARTESIAN_POINT ( 'NONE',  ( -12.50411668335183002, -6.909003531208875337, 33.74317678317729019 ) ) ;
#3317 = B_SPLINE_CURVE_WITH_KNOTS ( 'NONE', 3,
 ( #688, #4365, #3564, #3938, #3961, #733, #34, #1874, #2896, #1480, #3653, #4340, #1127, #2541, #3285, #1155 ),
 .UNSPECIFIED., .F., .F.,
 ( 4, 2, 2, 2, 2, 2, 2, 4 ),
 ( 0.004723219286513068334, 0.006427450678611836346, 0.007279566374661219051, 0.008131682070710601756, 0.008557739918735294410, 0.008983797766759987063, 0.009835913462809368901, 0.01154014485490813431 ),
 .UNSPECIFIED. ) ;
#3318 = VECTOR ( 'NONE', #1614, 1000.000000000000000 ) ;
#3319 = EDGE_CURVE ( 'NONE', #3535, #3784, #4247, .T. ) ;
#3320 = CIRCLE ( 'NONE', #4524, 0.7500000000000006661 ) ;
#3321 = ORIENTED_EDGE ( 'NONE', *, *, #1091, .T. ) ;
#3322 = CYLINDRICAL_SURFACE ( 'NONE', #3579, 0.7499999999999997780 ) ;
#3323 = DIRECTION ( 'NONE',  ( -8.673617379884027583E-16, -1.000000000000000000, 0.000000000000000000 ) ) ;
#3324 = VECTOR ( 'NONE', #2740, 1000.000000000000000 ) ;
#3325 = CARTESIAN_POINT ( 'NONE',  ( 14.00306357353840880, 2.843936418111722819, 34.04970046675368422 ) ) ;
#3326 = VERTEX_POINT ( 'NONE', #1701 ) ;
#3327 = ORIENTED_EDGE ( 'NONE', *, *, #3804, .T. ) ;
#3328 = ITEM_DEFINED_TRANSFORMATION ( 'NONE', 'NONE', #2591,  #4483 ) ;
#3329 = CARTESIAN_POINT ( 'NONE',  ( -13.30083885052560788, 5.220168816630788022, 37.25360547957401280 ) ) ;
#3330 = DIRECTION ( 'NONE',  ( 0.000000000000000000, 0.000000000000000000, -1.000000000000000000 ) ) ;
#3331 = ORIENTED_EDGE ( 'NONE', *, *, #467, .T. ) ;
#3332 = DIRECTION ( 'NONE',  ( 0.000000000000000000, 0.000000000000000000, -1.000000000000000000 ) ) ;
#3333 = CARTESIAN_POINT ( 'NONE',  ( -6.869994990996018736, 6.397500832047212427, 18.40096039353565160 ) ) ;
#3334 = CARTESIAN_POINT ( 'NONE',  ( 14.99250723456195544, 7.151597986548670072, 31.86762445358908735 ) ) ;
#3335 = CARTESIAN_POINT ( 'NONE',  ( -14.28159961045932214, -0.4665338100600365245, 35.41802149249647158 ) ) ;
#3336 = CARTESIAN_POINT ( 'NONE',  ( -12.37116712624658454, 7.147500832047209762, 18.40096039353565160 ) ) ;
#3337 = CARTESIAN_POINT ( 'NONE',  ( -3.573749999999998650, 0.000000000000000000, 11.11249999999999893 ) ) ;
#3338 = ADVANCED_FACE ( 'NONE', ( #2023 ), #3144, .F. ) ;
#3339 = EDGE_LOOP ( 'NONE', ( #1906, #2037, #3075, #1071 ) ) ;
#3340 = DIRECTION ( 'NONE',  ( 0.000000000000000000, 0.000000000000000000, 1.000000000000000000 ) ) ;
#3341 = CARTESIAN_POINT ( 'NONE',  ( -13.66280854539549772, -4.179239825960909371, 37.66764907019537389 ) ) ;
#3342 = ORIENTED_EDGE ( 'NONE', *, *, #424, .F. ) ;
#3343 = CARTESIAN_POINT ( 'NONE',  ( 14.17609414618484998, -1.787581051912757957, 28.76652967853488008 ) ) ;
#3344 = DIRECTION ( 'NONE',  ( -0.000000000000000000, -0.000000000000000000, 1.000000000000000000 ) ) ;
#3345 = CARTESIAN_POINT ( 'NONE',  ( -17.48249276543803532, -7.143402013451323640, 31.86762445358908735 ) ) ;
#3346 = ORIENTED_EDGE ( 'NONE', *, *, #1966, .T. ) ;
#3347 = EDGE_LOOP ( 'NONE', ( #2790, #4360, #3628, #3955 ) ) ;
#3348 = DIRECTION ( 'NONE',  ( 1.000000000000000000, 0.000000000000000000, 0.000000000000000000 ) ) ;
#3349 = EDGE_CURVE ( 'NONE', #849, #4649, #2330, .T. ) ;
#3350 = VERTEX_POINT ( 'NONE', #1679 ) ;
#3351 = AXIS2_PLACEMENT_3D ( 'NONE', #2876, #104, #554 ) ;
#3352 = CARTESIAN_POINT ( 'NONE',  ( 12.27079937262106668, 7.323080895278853752, 17.41529878742303694 ) ) ;
#3353 = EDGE_CURVE ( 'NONE', #3260, #209, #3182, .T. ) ;
#3354 = PLANE ( 'NONE',  #69 ) ;
#3355 = CARTESIAN_POINT ( 'NONE',  ( -14.28749276543804569, 0.2413016096126177623, 35.44137445358909133 ) ) ;
#3356 = CARTESIAN_POINT ( 'NONE',  ( 7.234561953626996335E-06, 0.004097986548672528061, 17.16762445358907385 ) ) ;
#3357 = EDGE_CURVE ( 'NONE', #1713, #3326, #3612, .T. ) ;
#3358 = APPLICATION_CONTEXT ( 'automotive_design' ) ;
#3359 = ORIENTED_EDGE ( 'NONE', *, *, #2432, .F. ) ;
#3360 = DIRECTION ( 'NONE',  ( -0.000000000000000000, -0.000000000000000000, -1.000000000000000000 ) ) ;
#3361 = AXIS2_PLACEMENT_3D ( 'NONE', #1313, #945, #1012 ) ;
#3362 = CARTESIAN_POINT ( 'NONE',  ( 14.28750723456195360, 0.2382004874472088418, 28.29387445358909403 ) ) ;
#3363 =( BOUNDED_CURVE ( )  B_SPLINE_CURVE ( 3, ( #4048, #4477, #3717, #1892 ),
 .UNSPECIFIED., .F., .F. ) 
 B_SPLINE_CURVE_WITH_KNOTS ( ( 4, 4 ),
 ( 3.141592653589793116, 4.712388980384689674 ),
 .UNSPECIFIED. ) 
 CURVE ( )  GEOMETRIC_REPRESENTATION_ITEM ( )  RATIONAL_B_SPLINE_CURVE ( ( 1.000000000000000000, 0.8047378541243649375, 0.8047378541243649375, 1.000000000000000000 ) ) 
 REPRESENTATION_ITEM ( '' )  );
#3364 = VERTEX_POINT ( 'NONE', #2520 ) ;
#3365 = PLANE ( 'NONE',  #2824 ) ;
#3366 = EDGE_CURVE ( 'NONE', #1488, #3260, #1895, .T. ) ;
#3367 = AXIS2_PLACEMENT_3D ( 'NONE', #4092, #3412, #2670 ) ;
#3368 = CYLINDRICAL_SURFACE ( 'NONE', #3544, 0.7500000000000006661 ) ;
#3369 = VECTOR ( 'NONE', #4267, 1000.000000000000000 ) ;
#3370 = ORIENTED_EDGE ( 'NONE', *, *, #3080, .T. ) ;
#3371 = EDGE_LOOP ( 'NONE', ( #1735, #3979, #1756, #1185 ) ) ;
#3372 = CARTESIAN_POINT ( 'NONE',  ( 8.370007234561951392, 0.004097986548671627739, 31.86762445358908735 ) ) ;
#3373 = CARTESIAN_POINT ( 'NONE',  ( -12.30670969789281699, -7.253995209643718134, 17.49673779855212885 ) ) ;
#3374 = EDGE_CURVE ( 'NONE', #3946, #4385, #1222, .T. ) ;
#3375 = ADVANCED_FACE ( 'NONE', ( #4272 ), #2108, .T. ) ;
#3376 = ORIENTED_EDGE ( 'NONE', *, *, #527, .F. ) ;
#3377 = CIRCLE ( 'NONE', #533, 3.573750000000000426 ) ;
#3378 = DIRECTION ( 'NONE',  ( 1.000000000000000000, -8.673617379884035472E-17, 0.000000000000000000 ) ) ;
#3379 = CARTESIAN_POINT ( 'NONE',  ( -8.369994990996012518, 7.147500832047212427, 32.36596039353565857 ) ) ;
#3380 = CARTESIAN_POINT ( 'NONE',  ( 12.50412892691776712, 6.913102349804759683, 34.24151272312386141 ) ) ;
#3381 = DIRECTION ( 'NONE',  ( -1.000000000000000000, 0.000000000000000000, 0.000000000000000000 ) ) ;
#3382 = ORIENTED_EDGE ( 'NONE', *, *, #4295, .F. ) ;
#3383 = FACE_OUTER_BOUND ( 'NONE', #4303, .T. ) ;
#3384 = AXIS2_PLACEMENT_3D ( 'NONE', #1683, #3486, #3869 ) ;
#3385 = CARTESIAN_POINT ( 'NONE',  ( -3.749994990996019517, 3.750000832047212906, 3.790960393535649064 ) ) ;
#3386 = EDGE_CURVE ( 'NONE', #1408, #1899, #1067, .T. ) ;
#3387 = AXIS2_PLACEMENT_3D ( 'NONE', #461, #2500, #3943 ) ;
#3388 = ORIENTED_EDGE ( 'NONE', *, *, #1589, .F. ) ;
#3389 = DIRECTION ( 'NONE',  ( -1.076498916035107621E-16, -1.000000000000000000, -8.841607930564763213E-17 ) ) ;
#3390 = CARTESIAN_POINT ( 'NONE',  ( -3.573742765438046476, 0.004097986548672528061, 17.16762445358907385 ) ) ;
#3391 = PRODUCT_DEFINITION_CONTEXT ( 'detailed design', #1357, 'design' ) ;
#3392 = LINE ( 'NONE', #170, #3318 ) ;
#3393 = AXIS2_PLACEMENT_3D ( 'NONE', #4011, #2619, #530 ) ;
#3394 = LINE ( 'NONE', #1615, #3583 ) ;
#3395 = ADVANCED_FACE ( 'NONE', ( #389 ), #4630, .T. ) ;
#3396 = VERTEX_POINT ( 'NONE', #343 ) ;
#3397 = EDGE_CURVE ( 'NONE', #1657, #98, #2474, .T. ) ;
#3398 = EDGE_LOOP ( 'NONE', ( #3271, #4026, #823, #4241 ) ) ;
#3399 = CONTEXT_DEPENDENT_SHAPE_REPRESENTATION ( #290, #2046 ) ;
#3400 = CARTESIAN_POINT ( 'NONE',  ( 14.00286243054562085, 2.840792968600885704, 30.18522767438163967 ) ) ;
#3401 = CARTESIAN_POINT ( 'NONE',  ( 17.28000050552179445, -2.539999999999999591, 17.28000050552179445 ) ) ;
#3402 = EDGE_CURVE ( 'NONE', #21, #4040, #1787, .T. ) ;
#3403 = VERTEX_POINT ( 'NONE', #1831 ) ;
#3404 = CARTESIAN_POINT ( 'NONE',  ( 3.573749999999998650, 4.376581498452851814E-16, 1.587499999999999467 ) ) ;
#3405 = DIRECTION ( 'NONE',  ( 0.000000000000000000, 1.000000000000000000, -0.000000000000000000 ) ) ;
#3406 = DIRECTION ( 'NONE',  ( -1.000000000000000000, 1.076498916035107744E-16, 0.000000000000000000 ) ) ;
#3407 = DIRECTION ( 'NONE',  ( 0.000000000000000000, -0.000000000000000000, -1.000000000000000000 ) ) ;
#3408 = CARTESIAN_POINT ( 'NONE',  ( 2.316727177394500794E-17, 0.000000000000000000, 11.11249999999999893 ) ) ;
#3409 = CARTESIAN_POINT ( 'NONE',  ( 3.750000000000000000, 3.750000000000000000, 146.2500000000000000 ) ) ;
#3410 = STYLED_ITEM ( 'NONE', ( #1382 ), #363 ) ;
#3411 = VERTEX_POINT ( 'NONE', #4298 ) ;
#3412 = DIRECTION ( 'NONE',  ( -1.000000000000000000, 1.076498916035107744E-16, 0.000000000000000000 ) ) ;
#3413 = CARTESIAN_POINT ( 'NONE',  ( 14.17558134697462968, 1.799572313586632610, 28.76893179367983677 ) ) ;
#3414 = VECTOR ( 'NONE', #3916, 1000.000000000000000 ) ;
#3415 = SHAPE_REPRESENTATION ( 'Part 131_Varsay\X2\0131\X0\lan', ( #4483 ), #4021 ) ;
#3416 = ORIENTED_EDGE ( 'NONE', *, *, #747, .F. ) ;
#3417 = CARTESIAN_POINT ( 'NONE',  ( -13.87981781320283226, 3.389924195623678305, 33.52105921454751325 ) ) ;
#3418 = CARTESIAN_POINT ( 'NONE',  ( -12.37116712624658454, -7.897499167952782173, 17.65096039353565160 ) ) ;
#3419 = CARTESIAN_POINT ( 'NONE',  ( 17.78000050552179445, -10.16000000000000014, 10.16000050552179701 ) ) ;
#3420 = ORIENTED_EDGE ( 'NONE', *, *, #2659, .T. ) ;
#3421 = EDGE_LOOP ( 'NONE', ( #157, #2116, #3445, #3105, #3184 ) ) ;
#3422 = DIRECTION ( 'NONE',  ( -1.000000000000000000, 0.000000000000000000, 0.000000000000000000 ) ) ;
#3423 = DIRECTION ( 'NONE',  ( -9.517981353260378315E-33, -8.841607930564763213E-17, 1.000000000000000000 ) ) ;
#3424 = EDGE_CURVE ( 'NONE', #2245, #4121, #607, .T. ) ;
#3425 = ORIENTED_EDGE ( 'NONE', *, *, #1625, .T. ) ;
#3426 = CARTESIAN_POINT ( 'NONE',  ( 2.540000505521796015, -2.539999999999999591, 17.78000050552179445 ) ) ;
#3427 = DIRECTION ( 'NONE',  ( -1.000000000000000000, 1.076498916035107621E-16, 0.000000000000000000 ) ) ;
#3428 = EDGE_CURVE ( 'NONE', #4575, #2026, #1080, .T. ) ;
#3429 = FACE_OUTER_BOUND ( 'NONE', #3859, .T. ) ;
#3430 = CARTESIAN_POINT ( 'NONE',  ( -14.24230335822356430, 1.160144388813159733, 35.25732888177847713 ) ) ;
#3431 = CARTESIAN_POINT ( 'NONE',  ( 14.28750723456195537, 0.004097986548674278397, 17.15262445358908039 ) ) ;
#3432 = MANIFOLD_SOLID_BREP ( 'Ölçek1', #638 ) ;
#3433 = VECTOR ( 'NONE', #1344, 1000.000000000000000 ) ;
#3434 = DIRECTION ( 'NONE',  ( 0.000000000000000000, 0.000000000000000000, 1.000000000000000000 ) ) ;
#3435 = ORIENTED_EDGE ( 'NONE', *, *, #2752, .F. ) ;
#3436 = LINE ( 'NONE', #111, #2609 ) ;
#3437 = ORIENTED_EDGE ( 'NONE', *, *, #2504, .T. ) ;
#3438 = DIRECTION ( 'NONE',  ( -1.076498916035107621E-16, 1.000000000000000000, 0.000000000000000000 ) ) ;
#3439 = VECTOR ( 'NONE', #4382, 1000.000000000000000 ) ;
#3440 = B_SPLINE_CURVE_WITH_KNOTS ( 'NONE', 3,
 ( #3499, #3546, #3914, #3844, #2448, #4580, #270, #2129, #598, #2470, #1323, #2043, #4176, #3863, #1785, #1697, #1366, #2422, #293, #1740, #623, #2736, #4269, #1717 ),
 .UNSPECIFIED., .F., .F.,
 ( 4, 2, 2, 2, 2, 2, 2, 2, 2, 2, 2, 4 ),
 ( 0.01136174788562026999, 0.01278160237203085359, 0.01420145685844143545, 0.01562131134485201904, 0.01633123858805730563, 0.01704116583126259049, 0.01775109307446787882, 0.01846102031767316368, 0.01988087480408372298, 0.02059080204728900437, 0.02130072929049427882, 0.02272058377690481731 ),
 .UNSPECIFIED. ) ;
#3441 = ORIENTED_EDGE ( 'NONE', *, *, #1836, .T. ) ;
#3442 = DIRECTION ( 'NONE',  ( 0.000000000000000000, 0.000000000000000000, 1.000000000000000000 ) ) ;
#3443 = DIRECTION ( 'NONE',  ( 0.000000000000000000, 0.000000000000000000, 1.000000000000000000 ) ) ;
#3444 = EDGE_LOOP ( 'NONE', ( #1691, #1474, #1173, #3882, #752 ) ) ;
#3445 = ORIENTED_EDGE ( 'NONE', *, *, #810, .T. ) ;
#3446 = CIRCLE ( 'NONE', #2235, 0.5000000000000000000 ) ;
#3447 = DIRECTION ( 'NONE',  ( 1.000000000000000000, 0.000000000000000000, 0.000000000000000000 ) ) ;
#3448 = EDGE_CURVE ( 'NONE', #4095, #566, #2543, .T. ) ;
#3449 = UNCERTAINTY_MEASURE_WITH_UNIT (LENGTH_MEASURE( 1.000000000000000082E-05 ), #2993, 'distance_accuracy_value', 'NONE');
#3450 = ORIENTED_EDGE ( 'NONE', *, *, #2895, .F. ) ;
#3451 = AXIS2_PLACEMENT_3D ( 'NONE', #3984, #2539, #1457 ) ;
#3452 = FACE_OUTER_BOUND ( 'NONE', #794, .T. ) ;
#3453 = CARTESIAN_POINT ( 'NONE',  ( -8.427206011669754915, 3.330701692678835979, 88.04858484712475786 ) ) ;
#3454 = APPLICATION_CONTEXT ( 'automotive_design' ) ;
#3455 = CARTESIAN_POINT ( 'NONE',  ( -13.86245963902841716, -3.459327043890196407, 33.29303758927057544 ) ) ;
#3456 = CARTESIAN_POINT ( 'NONE',  ( 10.16000050552179701, -13.73374999999999879, 10.16000050552179701 ) ) ;
#3457 = CARTESIAN_POINT ( 'NONE',  ( 12.37117936981251987, 7.151597986548670072, 31.86762445358908735 ) ) ;
#3458 = EDGE_CURVE ( 'NONE', #1283, #2998, #2397, .T. ) ;
#3459 = CARTESIAN_POINT ( 'NONE',  ( -13.83332089671217524, -3.569652013451325878, 31.63186830820603745 ) ) ;
#3460 = VERTEX_POINT ( 'NONE', #2992 ) ;
#3461 = AXIS2_PLACEMENT_3D ( 'NONE', #63, #1835, #347 ) ;
#3462 = LINE ( 'NONE', #3195, #2364 ) ;
#3463 = ORIENTED_EDGE ( 'NONE', *, *, #2001, .T. ) ;
#3464 = CARTESIAN_POINT ( 'NONE',  ( 14.28750723456195537, 0.004097986548674278397, 28.29387445358909403 ) ) ;
#3465 = ORIENTED_EDGE ( 'NONE', *, *, #2940, .T. ) ;
#3466 = EDGE_CURVE ( 'NONE', #98, #1569, #2559, .T. ) ;
#3467 = DIRECTION ( 'NONE',  ( 0.000000000000000000, 0.000000000000000000, 1.000000000000000000 ) ) ;
#3468 = B_SPLINE_CURVE_WITH_KNOTS ( 'NONE', 3,
 ( #2447, #3545, #575, #3455, #3479, #248, #3139, #3094, #4533, #3189, #1322, #269, #2376, #4268, #3862, #3821, #3120, #3498 ),
 .UNSPECIFIED., .F., .F.,
 ( 4, 2, 2, 2, 2, 2, 2, 2, 4 ),
 ( 0.01682638914732820234, 0.01752717873359113318, 0.01822796831985406055, 0.01892875790611699138, 0.01962954749237991875, 0.02033033707864284959, 0.02103112666490578042, 0.02173191625116870779, 0.02243270583743163862 ),
 .UNSPECIFIED. ) ;
#3469 = ADVANCED_FACE ( 'NONE', ( #2307 ), #4104, .F. ) ;
#3470 = CARTESIAN_POINT ( 'NONE',  ( 8.370007234561949616, -6.393402013451324528, 3.292624453589076960 ) ) ;
#3471 = VERTEX_POINT ( 'NONE', #503 ) ;
#3472 = VERTEX_POINT ( 'NONE', #1949 ) ;
#3473 = FILL_AREA_STYLE_COLOUR ( '', #3021 ) ;
#3474 = ORIENTED_EDGE ( 'NONE', *, *, #259, .T. ) ;
#3475 = CARTESIAN_POINT ( 'NONE',  ( 2.540000505521796015, -3.039999999999999147, 17.28000050552179445 ) ) ;
#3476 = DIRECTION ( 'NONE',  ( 0.000000000000000000, 0.000000000000000000, -1.000000000000000000 ) ) ;
#3477 = VECTOR ( 'NONE', #2263, 1000.000000000000000 ) ;
#3478 = SHAPE_REPRESENTATION_RELATIONSHIP ( 'NONE' , 'NONE' ,  #2171, #1632 ) ;
#3479 = CARTESIAN_POINT ( 'NONE',  ( -13.87980917377075585, -3.389965183367340096, 33.52105365422744399 ) ) ;
#3480 = DIRECTION ( 'NONE',  ( 1.000000000000000000, 0.000000000000000000, 0.000000000000000000 ) ) ;
#3481 = LINE ( 'NONE', #4177, #3226 ) ;
#3482 = VECTOR ( 'NONE', #1660, 1000.000000000000000 ) ;
#3483 = CARTESIAN_POINT ( 'NONE',  ( -14.17571295649602980, -1.794442765457400224, 29.26658434350617810 ) ) ;
#3484 = DIRECTION ( 'NONE',  ( -1.000000000000000000, 0.000000000000000000, 0.000000000000000000 ) ) ;
#3485 = EDGE_LOOP ( 'NONE', ( #2705, #1584, #1598, #1845 ) ) ;
#3486 = DIRECTION ( 'NONE',  ( 0.000000000000000000, 0.000000000000000000, 1.000000000000000000 ) ) ;
#3487 = CIRCLE ( 'NONE', #1832, 14.28750000000000142 ) ;
#3488 = EDGE_CURVE ( 'NONE', #4203, #195, #3008, .T. ) ;
#3489 = VERTEX_POINT ( 'NONE', #3404 ) ;
#3490 = DIRECTION ( 'NONE',  ( 0.000000000000000000, 0.000000000000000000, 1.000000000000000000 ) ) ;
#3491 = AXIS2_PLACEMENT_3D ( 'NONE', #3623, #3274, #3642 ) ;
#3492 = CARTESIAN_POINT ( 'NONE',  ( -12.37116712624657033, 7.147500832047212427, 32.36596039353565857 ) ) ;
#3493 = ORIENTED_EDGE ( 'NONE', *, *, #1449, .T. ) ;
#3494 = EDGE_LOOP ( 'NONE', ( #3580, #3346, #110 ) ) ;
#3495 = CARTESIAN_POINT ( 'NONE',  ( 12.25345478699094670, -6.586249999999999716, 8.066546224052645542 ) ) ;
#3496 = VERTEX_POINT ( 'NONE', #1624 ) ;
#3497 =( LENGTH_UNIT ( ) NAMED_UNIT ( * ) SI_UNIT ( .MILLI., .METRE. ) );
#3498 = CARTESIAN_POINT ( 'NONE',  ( -14.28749499099602005, 8.320472117659611842E-07, 35.93971039353566255 ) ) ;
#3499 = CARTESIAN_POINT ( 'NONE',  ( 14.28750500900398279, 8.320472145597748469E-07, 39.51346039353565942 ) ) ;
#3500 = EDGE_CURVE ( 'NONE', #4121, #4397, #1550, .T. ) ;
#3501 = EDGE_CURVE ( 'NONE', #1729, #2867, #781, .T. ) ;
#3502 = CARTESIAN_POINT ( 'NONE',  ( 14.00316917680643947, -2.839330532674458674, 34.54879557223570430 ) ) ;
#3503 = CARTESIAN_POINT ( 'NONE',  ( 11.96600771949147735, -7.803534059577478033, 17.15262445358908039 ) ) ;
#3504 = ORIENTED_EDGE ( 'NONE', *, *, #1240, .T. ) ;
#3505 = CARTESIAN_POINT ( 'NONE',  ( 13.73375050552179744, -10.16000000000000014, 17.78000050552179445 ) ) ;
#3506 = DIRECTION ( 'NONE',  ( 0.000000000000000000, -1.000000000000000000, 0.000000000000000000 ) ) ;
#3507 = ORIENTED_EDGE ( 'NONE', *, *, #3397, .T. ) ;
#3508 = PRODUCT_DEFINITION_SHAPE ( 'NONE', 'NONE',  #14 ) ;
#3509 = DIRECTION ( 'NONE',  ( 0.000000000000000000, 0.000000000000000000, 1.000000000000000000 ) ) ;
#3510 = ORIENTED_EDGE ( 'NONE', *, *, #3789, .F. ) ;
#3511 = EDGE_LOOP ( 'NONE', ( #2048, #1616, #3757, #4538 ) ) ;
#3512 = ADVANCED_FACE ( 'NONE', ( #3306, #2944 ), #831, .T. ) ;
#3513 = DIRECTION ( 'NONE',  ( -0.000000000000000000, -0.000000000000000000, -1.000000000000000000 ) ) ;
#3514 = EDGE_LOOP ( 'NONE', ( #4264, #1774, #3388, #685 ) ) ;
#3515 = CYLINDRICAL_SURFACE ( 'NONE', #4488, 0.7500000000000006661 ) ;
#3516 = CARTESIAN_POINT ( 'NONE',  ( 17.78000050552179800, -17.28000000000000114, 17.78000050552179445 ) ) ;
#3517 = CARTESIAN_POINT ( 'NONE',  ( -8.423113034125059073, 3.330708095193576579, 23.81500000000000128 ) ) ;
#3518 = ADVANCED_FACE ( 'NONE', ( #481 ), #223, .T. ) ;
#3519 = CARTESIAN_POINT ( 'NONE',  ( 17.28000050552179445, -3.039999999999999591, 17.28000050552179445 ) ) ;
#3520 = CARTESIAN_POINT ( 'NONE',  ( 14.28750500900398279, 8.320472145597748469E-07, 39.51346039353565942 ) ) ;
#3521 = FILL_AREA_STYLE_COLOUR ( '', #2257 ) ;
#3522 = ADVANCED_FACE ( 'NONE', ( #1573 ), #4213, .F. ) ;
#3523 = CIRCLE ( 'NONE', #3451, 3.573749999999999538 ) ;
#3524 = CARTESIAN_POINT ( 'NONE',  ( 8.370005009003978813, -6.397499167952787502, 32.36596039353565857 ) ) ;
#3525 = CARTESIAN_POINT ( 'NONE',  ( -14.00273932899718687, -2.837234857420575018, 29.68761152008073267 ) ) ;
#3526 = CARTESIAN_POINT ( 'NONE',  ( -8.369994990996016071, 7.147500832047212427, 18.40096039353565160 ) ) ;
#3527 = LINE ( 'NONE', #326, #1687 ) ;
#3528 = CARTESIAN_POINT ( 'NONE',  ( 11.90639837545767499, -7.893402013451324528, 17.15262445358908039 ) ) ;
#3529 = AXIS2_PLACEMENT_3D ( 'NONE', #1273, #4512, #1924 ) ;
#3530 = ORIENTED_EDGE ( 'NONE', *, *, #4074, .T. ) ;
#3531 = DIRECTION ( 'NONE',  ( 1.000000000000000000, 0.000000000000000000, 0.000000000000000000 ) ) ;
#3532 = MECHANICAL_DESIGN_GEOMETRIC_PRESENTATION_REPRESENTATION (  '', ( #1581 ), #295 ) ;
#3533 = DIRECTION ( 'NONE',  ( 0.000000000000000000, -1.000000000000000000, 0.000000000000000000 ) ) ;
#3534 = ORIENTED_EDGE ( 'NONE', *, *, #1129, .T. ) ;
#3535 = VERTEX_POINT ( 'NONE', #247 ) ;
#3536 = DIRECTION ( 'NONE',  ( -0.000000000000000000, 0.000000000000000000, 1.000000000000000000 ) ) ;
#3537 = ADVANCED_FACE ( 'NONE', ( #1337 ), #1674, .T. ) ;
#3538 = VECTOR ( 'NONE', #155, 1000.000000000000000 ) ;
#3539 = ORIENTED_EDGE ( 'NONE', *, *, #20, .F. ) ;
#3540 = CYLINDRICAL_SURFACE ( 'NONE', #3807, 0.5000000000000004441 ) ;
#3541 = ORIENTED_EDGE ( 'NONE', *, *, #3253, .F. ) ;
#3542 = CARTESIAN_POINT ( 'NONE',  ( -13.87969794115237399, 3.394527399177292626, 30.71358080212464259 ) ) ;
#3543 = VECTOR ( 'NONE', #2648, 1000.000000000000000 ) ;
#3544 = AXIS2_PLACEMENT_3D ( 'NONE', #901, #4384, #446 ) ;
#3545 = CARTESIAN_POINT ( 'NONE',  ( -13.83332312227014604, -3.573749167952787076, 32.60162372824473209 ) ) ;
#3546 = CARTESIAN_POINT ( 'NONE',  ( 14.28750500900398279, -0.4808399327370302956, 39.51346039353565942 ) ) ;
#3547 = AXIS2_PLACEMENT_3D ( 'NONE', #3265, #2545, #37 ) ;
#3548 = DIRECTION ( 'NONE',  ( 0.000000000000000000, 0.000000000000000000, -1.000000000000000000 ) ) ;
#3549 = PRODUCT_DEFINITION_SHAPE ( 'NONE', 'NONE',  #3694 ) ;
#3550 = CARTESIAN_POINT ( 'NONE',  ( -12.18302572395950989, -7.464154356144206304, 17.78097603577003127 ) ) ;
#3551 = CARTESIAN_POINT ( 'NONE',  ( -9.549434556529077899E-17, -3.249382362871961689E-18, 18.74999999999999645 ) ) ;
#3552 = CARTESIAN_POINT ( 'NONE',  ( 3.040000505521796015, -2.540000000000000480, 2.540000505521796015 ) ) ;
#3553 = ORIENTED_EDGE ( 'NONE', *, *, #404, .F. ) ;
#3554 = CARTESIAN_POINT ( 'NONE',  ( 13.42338109688237502, -4.892394157346815931, 37.07949484329716938 ) ) ;
#3555 = LINE ( 'NONE', #4259, #332 ) ;
#3556 = ORIENTED_EDGE ( 'NONE', *, *, #2777, .F. ) ;
#3557 = ORIENTED_EDGE ( 'NONE', *, *, #3866, .F. ) ;
#3558 = AXIS2_PLACEMENT_3D ( 'NONE', #771, #353, #1798 ) ;
#3559 = VERTEX_POINT ( 'NONE', #3118 ) ;
#3560 = DIRECTION ( 'NONE',  ( 1.000000000000000000, 0.000000000000000000, 0.000000000000000000 ) ) ;
#3561 = ORIENTED_EDGE ( 'NONE', *, *, #4127, .T. ) ;
#3562 = CARTESIAN_POINT ( 'NONE',  ( 17.78000050552179445, -10.16000000000000014, 6.586250505521796583 ) ) ;
#3563 =( NAMED_UNIT ( * ) SI_UNIT ( $, .STERADIAN. ) SOLID_ANGLE_UNIT ( ) );
#3564 = CARTESIAN_POINT ( 'NONE',  ( -2.181621296273096533, -3.565902013451326180, -9.148124867462044563 ) ) ;
#3565 = CARTESIAN_POINT ( 'NONE',  ( 7.234561953626996335E-06, 0.004097986548672528061, 17.15262445358908039 ) ) ;
#3566 = EDGE_CURVE ( 'NONE', #44, #2368, #3795, .T. ) ;
#3567 = CARTESIAN_POINT ( 'NONE',  ( -14.17567608032355686, 1.794650183413384115, 29.26677597323998725 ) ) ;
#3568 = DIRECTION ( 'NONE',  ( -1.076498916035107621E-16, 1.000000000000000000, 0.000000000000000000 ) ) ;
#3569 = CARTESIAN_POINT ( 'NONE',  ( 3.152229664848242408, -3.565902013451327068, -10.04237554641092345 ) ) ;
#3570 = DIRECTION ( 'NONE',  ( -0.000000000000000000, -0.000000000000000000, 1.000000000000000000 ) ) ;
#3571 = VERTEX_POINT ( 'NONE', #976 ) ;
#3572 = CARTESIAN_POINT ( 'NONE',  ( 8.370005009003978813, 8.320472119090310841E-07, 32.36596039353565857 ) ) ;
#3573 =( GEOMETRIC_REPRESENTATION_CONTEXT ( 3 ) GLOBAL_UNCERTAINTY_ASSIGNED_CONTEXT ( ( #906 ) ) GLOBAL_UNIT_ASSIGNED_CONTEXT ( ( #574, #3069, #3138 ) ) REPRESENTATION_CONTEXT ( 'NONE', 'WORKASPACE' ) );
#3574 = CARTESIAN_POINT ( 'NONE',  ( 7.620007234561953169, 0.004097986548671708404, 31.86762445358909446 ) ) ;
#3575 = AXIS2_PLACEMENT_3D ( 'NONE', #345, #3918, #2854 ) ;
#3576 = ORIENTED_EDGE ( 'NONE', *, *, #3835, .F. ) ;
#3577 = ORIENTED_EDGE ( 'NONE', *, *, #828, .F. ) ;
#3578 = SURFACE_STYLE_FILL_AREA ( #2123 ) ;
#3579 = AXIS2_PLACEMENT_3D ( 'NONE', #3581, #4600, #1362 ) ;
#3580 = ORIENTED_EDGE ( 'NONE', *, *, #3741, .T. ) ;
#3581 = CARTESIAN_POINT ( 'NONE',  ( 6.870007234561952281, 12.08996809382683857, 17.90262445358908039 ) ) ;
#3582 = CARTESIAN_POINT ( 'NONE',  ( 12.37117936981251987, 7.151597986548668295, 17.15262445358908039 ) ) ;
#3583 = VECTOR ( 'NONE', #4120, 1000.000000000000000 ) ;
#3584 = DIRECTION ( 'NONE',  ( 0.9751221211376644993, 2.602085213965210642E-17, -0.2216683307736628805 ) ) ;
#3585 = DIRECTION ( 'NONE',  ( 0.000000000000000000, 1.000000000000000000, 0.000000000000000000 ) ) ;
#3586 = EDGE_CURVE ( 'NONE', #975, #2245, #268, .T. ) ;
#3587 = CARTESIAN_POINT ( 'NONE',  ( 3.040000505521796015, -17.28000000000000114, 17.28000050552179445 ) ) ;
#3588 = CARTESIAN_POINT ( 'NONE',  ( 7.234561953626996335E-06, 0.004097986548672528061, -10.04237554641092345 ) ) ;
#3589 = CARTESIAN_POINT ( 'NONE',  ( -12.35763252401195800, -7.171051608339699790, 18.18681329310062367 ) ) ;
#3590 = VECTOR ( 'NONE', #3360, 1000.000000000000000 ) ;
#3591 = CARTESIAN_POINT ( 'NONE',  ( 5.009003980371977336E-06, 8.320472128100606877E-07, 3.790960393535649064 ) ) ;
#3592 = CARTESIAN_POINT ( 'NONE',  ( 17.28000050552179800, -17.28000000000000114, 17.28000050552179445 ) ) ;
#3593 = EDGE_CURVE ( 'NONE', #3571, #4067, #3841, .T. ) ;
#3594 = DIRECTION ( 'NONE',  ( 0.000000000000000000, 0.000000000000000000, 1.000000000000000000 ) ) ;
#3595 = ADVANCED_FACE ( 'NONE', ( #2063 ), #514, .T. ) ;
#3596 = ORIENTED_EDGE ( 'NONE', *, *, #1849, .T. ) ;
#3597 = CARTESIAN_POINT ( 'NONE',  ( -8.369992765438045268, -7.893402013451322752, 17.90262445358908039 ) ) ;
#3598 = CARTESIAN_POINT ( 'NONE',  ( -14.16477841556124062, -1.878420794868401300, 38.76682706999738315 ) ) ;
#3599 = EDGE_CURVE ( 'NONE', #3603, #116, #4577, .T. ) ;
#3600 =( REPRESENTATION_RELATIONSHIP ('NONE','NONE', #4401, #2003 ) REPRESENTATION_RELATIONSHIP_WITH_TRANSFORMATION ( #1618 )SHAPE_REPRESENTATION_RELATIONSHIP( ) );
#3601 = DIRECTION ( 'NONE',  ( -8.673617379884035472E-17, 1.000000000000000000, 0.000000000000000000 ) ) ;
#3602 = ORIENTED_EDGE ( 'NONE', *, *, #2080, .F. ) ;
#3603 = VERTEX_POINT ( 'NONE', #637 ) ;
#3604 = AXIS2_PLACEMENT_3D ( 'NONE', #369, #2247, #3291 ) ;
#3605 = CARTESIAN_POINT ( 'NONE',  ( -12.76993684346950708, 6.415192739153763313, 35.06135232679011438 ) ) ;
#3606 = ORIENTED_EDGE ( 'NONE', *, *, #3734, .F. ) ;
#3607 = ORIENTED_EDGE ( 'NONE', *, *, #3929, .F. ) ;
#3608 = CARTESIAN_POINT ( 'NONE',  ( 3.750005009003979595, 3.750000832047212906, 17.65096039353565160 ) ) ;
#3609 = APPLICATION_PROTOCOL_DEFINITION ( 'draft international standard', 'automotive_design', 1998, #3358 ) ;
#3610 = CARTESIAN_POINT ( 'NONE',  ( 12.87896255196901407, 6.196505624857743477, 35.46704985752300843 ) ) ;
#3611 = CARTESIAN_POINT ( 'NONE',  ( 8.370005009003978813, -6.397499167952786614, 17.65096039353565160 ) ) ;
#3612 = LINE ( 'NONE', #1856, #3089 ) ;
#3613 = CARTESIAN_POINT ( 'NONE',  ( -12.37116712624659343, -7.147499167952783061, 18.29228486772271722 ) ) ;
#3614 = FACE_OUTER_BOUND ( 'NONE', #4526, .T. ) ;
#3615 = DIRECTION ( 'NONE',  ( -1.000000000000000000, 0.000000000000000000, 0.000000000000000000 ) ) ;
#3616 = AXIS2_PLACEMENT_3D ( 'NONE', #1030, #936, #4201 ) ;
#3617 = DIRECTION ( 'NONE',  ( -1.000000000000000000, 1.076498916035107621E-16, 0.000000000000000000 ) ) ;
#3618 = VECTOR ( 'NONE', #2640, 1000.000000000000000 ) ;
#3619 = CARTESIAN_POINT ( 'NONE',  ( -9.549434556529077899E-17, 3.750000000000000000, 3.749999999999995559 ) ) ;
#3620 = VERTEX_POINT ( 'NONE', #2691 ) ;
#3621 = DIRECTION ( 'NONE',  ( -0.000000000000000000, -0.000000000000000000, -1.000000000000000000 ) ) ;
#3622 = CARTESIAN_POINT ( 'NONE',  ( -13.11702252608348651, -5.661701175589295865, 36.23092228855526997 ) ) ;
#3623 = CARTESIAN_POINT ( 'NONE',  ( 7.234561953626996335E-06, 0.004097986548672528061, 3.292624453589077405 ) ) ;
#3624 = ORIENTED_EDGE ( 'NONE', *, *, #4635, .T. ) ;
#3625 = VERTEX_POINT ( 'NONE', #2084 ) ;
#3626 = DIRECTION ( 'NONE',  ( 0.000000000000000000, 0.000000000000000000, -1.000000000000000000 ) ) ;
#3627 = MECHANICAL_DESIGN_GEOMETRIC_PRESENTATION_REPRESENTATION (  '', ( #3410 ), #621 ) ;
#3628 = ORIENTED_EDGE ( 'NONE', *, *, #4084, .F. ) ;
#3629 = ORIENTED_EDGE ( 'NONE', *, *, #2192, .T. ) ;
#3630 = CARTESIAN_POINT ( 'NONE',  ( -13.94802501356800661, 3.102887394450430047, 30.07232133647258010 ) ) ;
#3631 = CARTESIAN_POINT ( 'NONE',  ( 1.736892480400722638, -6.829291578281011077, -123.6290396064643602 ) ) ;
#3632 = CARTESIAN_POINT ( 'NONE',  ( 14.28750723456195537, 0.004097986548674278397, 39.01512445358908820 ) ) ;
#3633 = DIRECTION ( 'NONE',  ( -1.000000000000000000, -0.000000000000000000, -0.000000000000000000 ) ) ;
#3634 = CARTESIAN_POINT ( 'NONE',  ( 3.750000000000000000, 3.750000000000000000, 131.2499999999999716 ) ) ;
#3635 = CARTESIAN_POINT ( 'NONE',  ( -13.83332312227014427, 3.573750832047213777, 32.36596039353566567 ) ) ;
#3636 = ADVANCED_FACE ( 'NONE', ( #4219 ), #3861, .F. ) ;
#3637 = CARTESIAN_POINT ( 'NONE',  ( -14.24206744302798633, -1.154622011196222653, 35.25632758055221672 ) ) ;
#3638 = CARTESIAN_POINT ( 'NONE',  ( -8.369992765438045268, 0.004097986548673428382, 31.86762445358908735 ) ) ;
#3639 = ORIENTED_EDGE ( 'NONE', *, *, #4354, .T. ) ;
#3640 = FACE_BOUND ( 'NONE', #3485, .T. ) ;
#3641 = DIRECTION ( 'NONE',  ( 1.076498916035107621E-16, -1.000000000000000000, 0.000000000000000000 ) ) ;
#3642 = DIRECTION ( 'NONE',  ( 1.000000000000000000, 0.000000000000000000, 0.000000000000000000 ) ) ;
#3643 = ORIENTED_EDGE ( 'NONE', *, *, #3353, .F. ) ;
#3644 = SHAPE_DEFINITION_REPRESENTATION ( #3549, #3415 ) ;
#3645 = ORIENTED_EDGE ( 'NONE', *, *, #712, .F. ) ;
#3646 = CARTESIAN_POINT ( 'NONE',  ( -12.47853676740481887, 6.962653799640055929, 33.51726641232498594 ) ) ;
#3647 = CLOSED_SHELL ( 'NONE', ( #4435, #2785, #32, #4423, #2581, #1230, #1383, #4110, #4184, #2216, #2508, #1595, #1517, #573, #2374, #1784, #784, #3735, #2303, #2814, #2267, #3820, #4496, #2999, #2305, #3839, #2542, #1255, #2550, #90, #4644, #3518, #1013, #1905 ) ) ;
#3648 = AXIS2_PLACEMENT_3D ( 'NONE', #3016, #4462, #531 ) ;
#3649 = EDGE_LOOP ( 'NONE', ( #2033, #4436, #2951, #2234 ) ) ;
#3650 = DIRECTION ( 'NONE',  ( 1.000000000000000000, 0.000000000000000000, -0.000000000000000000 ) ) ;
#3651 = EDGE_CURVE ( 'NONE', #4134, #1870, #1295, .T. ) ;
#3652 = AXIS2_PLACEMENT_3D ( 'NONE', #2827, #444, #706 ) ;
#3653 = CARTESIAN_POINT ( 'NONE',  ( 0.7146566484001382058, -3.565902013451327957, -9.666548897786826799 ) ) ;
#3654 = AXIS2_PLACEMENT_3D ( 'NONE', #3638, #371, #4015 ) ;
#3655 = DIRECTION ( 'NONE',  ( 1.076498916035107744E-16, 1.000000000000000000, 0.000000000000000000 ) ) ;
#3656 = PRESENTATION_STYLE_ASSIGNMENT (( #4033 ) ) ;
#3657 = LINE ( 'NONE', #3266, #717 ) ;
#3658 = EDGE_CURVE ( 'NONE', #4593, #2966, #954, .T. ) ;
#3659 = LINE ( 'NONE', #434, #1132 ) ;
#3660 = CARTESIAN_POINT ( 'NONE',  ( 14.00317140236440849, -2.835233378172992591, 34.05045963228912598 ) ) ;
#3661 = FACE_OUTER_BOUND ( 'NONE', #707, .T. ) ;
#3662 = AXIS2_PLACEMENT_3D ( 'NONE', #3597, #2183, #2579 ) ;
#3663 = ORIENTED_EDGE ( 'NONE', *, *, #3599, .F. ) ;
#3664 = CARTESIAN_POINT ( 'NONE',  ( 5.009003980371977336E-06, 8.320472128100606877E-07, 17.65096039353565160 ) ) ;
#3665 = DIRECTION ( 'NONE',  ( 0.000000000000000000, 0.000000000000000000, 1.000000000000000000 ) ) ;
#3666 = VECTOR ( 'NONE', #78, 1000.000000000000000 ) ;
#3667 = EDGE_LOOP ( 'NONE', ( #1568, #3435, #1843, #3054, #196 ) ) ;
#3668 = DIRECTION ( 'NONE',  ( 1.000000000000000000, -1.076498916035107744E-16, -0.000000000000000000 ) ) ;
#3669 = LINE ( 'NONE', #2958, #1136 ) ;
#3670 = CARTESIAN_POINT ( 'NONE',  ( -6.869994990996020512, 6.397500832047212427, 17.65096039353565160 ) ) ;
#3671 = VERTEX_POINT ( 'NONE', #2373 ) ;
#3672 = CIRCLE ( 'NONE', #372, 3.573749999999999538 ) ;
#3673 = ORIENTED_EDGE ( 'NONE', *, *, #1333, .F. ) ;
#3674 = CARTESIAN_POINT ( 'NONE',  ( -13.60367840868947908, 4.371228564879502620, 38.02566532807935573 ) ) ;
#3675 = CARTESIAN_POINT ( 'NONE',  ( -11.96610561084410840, -7.803364663213757879, 17.15262445358908039 ) ) ;
#3676 = CARTESIAN_POINT ( 'NONE',  ( 14.12123511036389090, -2.182294823265078509, 29.52615613029221109 ) ) ;
#3677 = EDGE_CURVE ( 'NONE', #566, #1305, #71, .T. ) ;
#3678 = VERTEX_POINT ( 'NONE', #1651 ) ;
#3679 = CYLINDRICAL_SURFACE ( 'NONE', #3648, 0.5000000000000000000 ) ;
#3680 = FACE_OUTER_BOUND ( 'NONE', #3667, .T. ) ;
#3681 = CYLINDRICAL_SURFACE ( 'NONE', #3387, 7.147499999999999076 ) ;
#3682 = CIRCLE ( 'NONE', #1061, 1.499999999999999556 ) ;
#3683 = DIRECTION ( 'NONE',  ( 0.000000000000000000, 0.000000000000000000, 1.000000000000000000 ) ) ;
#3684 =( REPRESENTATION_RELATIONSHIP ('NONE','NONE', #4401, #1824 ) REPRESENTATION_RELATIONSHIP_WITH_TRANSFORMATION ( #2684 )SHAPE_REPRESENTATION_RELATIONSHIP( ) );
#3685 = ORIENTED_EDGE ( 'NONE', *, *, #2329, .T. ) ;
#3686 = DIRECTION ( 'NONE',  ( 0.000000000000000000, 0.000000000000000000, -1.000000000000000000 ) ) ;
#3687 = AXIS2_PLACEMENT_3D ( 'NONE', #1944, #3012, #3422 ) ;
#3688 = LINE ( 'NONE', #469, #2643 ) ;
#3689 = CYLINDRICAL_SURFACE ( 'NONE', #2495, 3.573749999999998650 ) ;
#3690 = ORIENTED_EDGE ( 'NONE', *, *, #303, .F. ) ;
#3691 = CARTESIAN_POINT ( 'NONE',  ( 14.20095123608300014, -1.580981516206518833, 28.65617994343129382 ) ) ;
#3692 = VECTOR ( 'NONE', #3423, 1000.000000000000000 ) ;
#3693 = LINE ( 'NONE', #2281, #2768 ) ;
#3694 = PRODUCT_DEFINITION ( 'UNKNOWN', '', #416, #2677 ) ;
#3695 = VECTOR ( 'NONE', #3126, 1000.000000000000000 ) ;
#3696 = DIRECTION ( 'NONE',  ( 1.000000000000000000, -1.076498916035107621E-16, -0.000000000000000000 ) ) ;
#3697 = ORIENTED_EDGE ( 'NONE', *, *, #3152, .T. ) ;
#3698 = EDGE_LOOP ( 'NONE', ( #2158, #4237, #3441, #1223 ) ) ;
#3699 = DIRECTION ( 'NONE',  ( 0.000000000000000000, 0.000000000000000000, 1.000000000000000000 ) ) ;
#3700 = ADVANCED_FACE ( 'NONE', ( #4531 ), #2615, .T. ) ;
#3701 = DIRECTION ( 'NONE',  ( 0.000000000000000000, 0.000000000000000000, 1.000000000000000000 ) ) ;
#3702 = ORIENTED_EDGE ( 'NONE', *, *, #4276, .T. ) ;
#3703 = DIRECTION ( 'NONE',  ( 0.000000000000000000, 0.000000000000000000, 1.000000000000000000 ) ) ;
#3704 = DIRECTION ( 'NONE',  ( 1.000000000000000000, 0.000000000000000000, 0.000000000000000000 ) ) ;
#3705 = DIRECTION ( 'NONE',  ( 0.000000000000000000, -1.000000000000000000, 0.000000000000000000 ) ) ;
#3706 = DIRECTION ( 'NONE',  ( 0.000000000000000000, -1.000000000000000000, 0.000000000000000000 ) ) ;
#3707 = CARTESIAN_POINT ( 'NONE',  ( 6.870005009003977925, 6.397500832047211539, 17.65096039353565160 ) ) ;
#3708 = AXIS2_PLACEMENT_3D ( 'NONE', #2653, #442, #1909 ) ;
#3709 = EDGE_CURVE ( 'NONE', #4134, #3312, #571, .T. ) ;
#3710 = EDGE_LOOP ( 'NONE', ( #2909, #472, #4169, #705 ) ) ;
#3711 = DIRECTION ( 'NONE',  ( -1.076498916035107621E-16, 1.000000000000000000, -0.000000000000000000 ) ) ;
#3712 = DIRECTION ( 'NONE',  ( 1.000000000000000000, 0.000000000000000000, 0.000000000000000000 ) ) ;
#3713 = FACE_OUTER_BOUND ( 'NONE', #702, .T. ) ;
#3714 = ORIENTED_EDGE ( 'NONE', *, *, #3319, .F. ) ;
#3715 = CYLINDRICAL_SURFACE ( 'NONE', #4409, 0.7499999999999997780 ) ;
#3716 = LINE ( 'NONE', #1192, #3751 ) ;
#3717 = CARTESIAN_POINT ( 'NONE',  ( 8.066546224052645542, -6.586249999999999716, 12.25345478699094670 ) ) ;
#3718 = EDGE_LOOP ( 'NONE', ( #2563, #1605, #4185, #1293, #4424, #751 ) ) ;
#3719 = ORIENTED_EDGE ( 'NONE', *, *, #3458, .T. ) ;
#3720 = CARTESIAN_POINT ( 'NONE',  ( -14.28749499099602005, 8.320472128100606877E-07, 39.51346039353565942 ) ) ;
#3721 = PRODUCT_DEFINITION_FORMATION_WITH_SPECIFIED_SOURCE ( 'ANY', '', #2825, .NOT_KNOWN. ) ;
#3722 = DIRECTION ( 'NONE',  ( -1.000000000000000000, 0.000000000000000000, 0.000000000000000000 ) ) ;
#3723 = ORIENTED_EDGE ( 'NONE', *, *, #260, .F. ) ;
#3724 =( NAMED_UNIT ( * ) SI_UNIT ( $, .STERADIAN. ) SOLID_ANGLE_UNIT ( ) );
#3725 = ADVANCED_FACE ( 'NONE', ( #3452 ), #1321, .T. ) ;
#3726 = CARTESIAN_POINT ( 'NONE',  ( 8.370007234561949616, 6.401597986548672736, 31.86762445358908735 ) ) ;
#3727 = CARTESIAN_POINT ( 'NONE',  ( 12.37117714425454551, 7.147500832047209762, 32.36596039353565857 ) ) ;
#3728 = DIRECTION ( 'NONE',  ( 1.000000000000000000, 0.000000000000000000, -0.000000000000000000 ) ) ;
#3729 = DIRECTION ( 'NONE',  ( 1.000000000000000000, -8.673617379884035472E-17, 0.000000000000000000 ) ) ;
#3730 = ORIENTED_EDGE ( 'NONE', *, *, #870, .T. ) ;
#3731 = DIRECTION ( 'NONE',  ( 1.000000000000000000, 0.000000000000000000, -0.000000000000000000 ) ) ;
#3732 = CIRCLE ( 'NONE', #3286, 4.762499999999999289 ) ;
#3733 = CARTESIAN_POINT ( 'NONE',  ( 14.24248549217296400, 1.158197531232292299, 28.47721150812772350 ) ) ;
#3734 = EDGE_CURVE ( 'NONE', #254, #3850, #3523, .T. ) ;
#3735 = ADVANCED_FACE ( 'NONE', ( #1409 ), #1387, .T. ) ;
#3736 = ADVANCED_FACE ( 'NONE', ( #2170 ), #757, .T. ) ;
#3737 = VERTEX_POINT ( 'NONE', #2127 ) ;
#3738 = CARTESIAN_POINT ( 'NONE',  ( 14.09194898772133975, -2.357612872106044311, 29.17542961446211081 ) ) ;
#3739 = CARTESIAN_POINT ( 'NONE',  ( -14.03250750257131152, 2.692405860157741415, 34.72743248988972198 ) ) ;
#3740 = EDGE_CURVE ( 'NONE', #1351, #2813, #1873, .T. ) ;
#3741 = EDGE_CURVE ( 'NONE', #3326, #4397, #4347, .T. ) ;
#3742 = LINE ( 'NONE', #1963, #1146 ) ;
#3743 = CARTESIAN_POINT ( 'NONE',  ( 14.28750723456195715, 0.2398388336121953790, 35.44137445358909133 ) ) ;
#3744 = ORIENTED_EDGE ( 'NONE', *, *, #2752, .T. ) ;
#3745 = VERTEX_POINT ( 'NONE', #3608 ) ;
#3746 = CONTEXT_DEPENDENT_SHAPE_REPRESENTATION ( #2150, #144 ) ;
#3747 = CYLINDRICAL_SURFACE ( 'NONE', #3687, 14.28750000000000142 ) ;
#3748 = CARTESIAN_POINT ( 'NONE',  ( 7.620005009003977037, 6.397500832047211539, 17.65096039353565160 ) ) ;
#3749 = EDGE_LOOP ( 'NONE', ( #1557, #3932 ) ) ;
#3750 = CARTESIAN_POINT ( 'NONE',  ( 7.620005009003978813, 8.320472119897684647E-07, 32.36596039353566567 ) ) ;
#3751 = VECTOR ( 'NONE', #492, 1000.000000000000000 ) ;
#3752 = CARTESIAN_POINT ( 'NONE',  ( 0.000000000000000000, 0.000000000000000000, 0.000000000000000000 ) ) ;
#3753 = LINE ( 'NONE', #2665, #292 ) ;
#3754 = CARTESIAN_POINT ( 'NONE',  ( -14.28159378806564206, 0.4743560429282985824, 35.41799410330143161 ) ) ;
#3755 = DIRECTION ( 'NONE',  ( -0.000000000000000000, -0.000000000000000000, -1.000000000000000000 ) ) ;
#3756 = LINE ( 'NONE', #536, #1647 ) ;
#3757 = ORIENTED_EDGE ( 'NONE', *, *, #2128, .T. ) ;
#3758 = LINE ( 'NONE', #3077, #1653 ) ;
#3759 = CIRCLE ( 'NONE', #1141, 3.573749999999998650 ) ;
#3760 = FACE_BOUND ( 'NONE', #382, .T. ) ;
#3761 = CIRCLE ( 'NONE', #1747, 14.28750000000000142 ) ;
#3762 = ORIENTED_EDGE ( 'NONE', *, *, #520, .T. ) ;
#3763 = DIRECTION ( 'NONE',  ( 0.000000000000000000, 1.000000000000000000, 0.000000000000000000 ) ) ;
#3764 = EDGE_CURVE ( 'NONE', #4454, #1093, #1762, .T. ) ;
#3765 = VECTOR ( 'NONE', #2112, 1000.000000000000000 ) ;
#3766 = CARTESIAN_POINT ( 'NONE',  ( 18.74250500900397753, 3.573750832047210224, 32.36596039353566567 ) ) ;
#3767 = AXIS2_PLACEMENT_3D ( 'NONE', #3750, #4437, #1600 ) ;
#3768 = CARTESIAN_POINT ( 'NONE',  ( 14.17575381291738523, 1.798219341900524348, 34.96710348429465398 ) ) ;
#3769 = EDGE_CURVE ( 'NONE', #1498, #1942, #665, .T. ) ;
#3770 = ORIENTED_EDGE ( 'NONE', *, *, #3741, .F. ) ;
#3771 = ORIENTED_EDGE ( 'NONE', *, *, #1763, .T. ) ;
#3772 = CARTESIAN_POINT ( 'NONE',  ( -14.26330390617519761, 0.9521795732501526777, 39.46544505580351370 ) ) ;
#3773 = UNCERTAINTY_MEASURE_WITH_UNIT (LENGTH_MEASURE( 1.000000000000000082E-05 ), #3497, 'distance_accuracy_value', 'NONE');
#3774 = VERTEX_POINT ( 'NONE', #1048 ) ;
#3775 = DIRECTION ( 'NONE',  ( -0.000000000000000000, -0.000000000000000000, -1.000000000000000000 ) ) ;
#3776 =( NAMED_UNIT ( * ) SI_UNIT ( $, .STERADIAN. ) SOLID_ANGLE_UNIT ( ) );
#3777 = CARTESIAN_POINT ( 'NONE',  ( -3.749994990996019961, 8.320472131353213394E-07, 17.65096039353565160 ) ) ;
#3778 = CARTESIAN_POINT ( 'NONE',  ( 13.66282078896143659, 4.183338644556793717, 38.16598501014196643 ) ) ;
#3779 = LINE ( 'NONE', #862, #7 ) ;
#3780 = CARTESIAN_POINT ( 'NONE',  ( -7.619994990996017847, 12.08587093932537826, 39.51346039353565232 ) ) ;
#3781 = ORIENTED_EDGE ( 'NONE', *, *, #3349, .F. ) ;
#3782 = CARTESIAN_POINT ( 'NONE',  ( 18.74250723456195189, 0.004097986548670510577, 31.86762445358909446 ) ) ;
#3783 = EDGE_CURVE ( 'NONE', #3774, #3559, #2869, .T. ) ;
#3784 = VERTEX_POINT ( 'NONE', #2194 ) ;
#3785 = CARTESIAN_POINT ( 'NONE',  ( 14.12134054576453934, 2.185513808779087963, 29.02736931185435054 ) ) ;
#3786 = CIRCLE ( 'NONE', #2278, 1.499999999999999556 ) ;
#3787 = ORIENTED_EDGE ( 'NONE', *, *, #2659, .F. ) ;
#3788 = DIRECTION ( 'NONE',  ( 0.000000000000000000, 1.000000000000000000, 0.000000000000000000 ) ) ;
#3789 = EDGE_CURVE ( 'NONE', #4140, #849, #4532, .T. ) ;
#3790 = CARTESIAN_POINT ( 'NONE',  ( 3.573749999999998650, 4.376581498452851814E-16, 11.11249999999999893 ) ) ;
#3791 = ORIENTED_EDGE ( 'NONE', *, *, #1316, .T. ) ;
#3792 = VERTEX_POINT ( 'NONE', #2513 ) ;
#3793 = EDGE_CURVE ( 'NONE', #3496, #4402, #1433, .T. ) ;
#3794 = ORIENTED_EDGE ( 'NONE', *, *, #1220, .F. ) ;
#3795 = LINE ( 'NONE', #2754, #3892 ) ;
#3796 = DIRECTION ( 'NONE',  ( 2.428612866367525618E-17, -1.000000000000000000, 0.000000000000000000 ) ) ;
#3797 = DIRECTION ( 'NONE',  ( -0.000000000000000000, 1.000000000000000000, 0.000000000000000000 ) ) ;
#3798 = CARTESIAN_POINT ( 'NONE',  ( 14.26329420569817685, 0.9536349444224723193, 39.46541283322252980 ) ) ;
#3799 = CARTESIAN_POINT ( 'NONE',  ( -3.573749999999998650, 0.000000000000000000, 11.11249999999999893 ) ) ;
#3800 = VECTOR ( 'NONE', #4631, 1000.000000000000000 ) ;
#3801 = ADVANCED_FACE ( 'NONE', ( #1781 ), #3209, .T. ) ;
#3802 = CARTESIAN_POINT ( 'NONE',  ( 13.83942688247485897, -3.550395471754214771, 32.83659103844913574 ) ) ;
#3803 = ORIENTED_EDGE ( 'NONE', *, *, #2552, .T. ) ;
#3804 = EDGE_CURVE ( 'NONE', #1869, #1569, #2145, .T. ) ;
#3805 = CARTESIAN_POINT ( 'NONE',  ( 11.90639837545767499, -7.893402013451324528, 17.15262445358908039 ) ) ;
#3806 = DIRECTION ( 'NONE',  ( 0.000000000000000000, 0.000000000000000000, -1.000000000000000000 ) ) ;
#3807 = AXIS2_PLACEMENT_3D ( 'NONE', #1169, #4265, #2083 ) ;
#3808 = VERTEX_POINT ( 'NONE', #4363 ) ;
#3809 = AXIS2_PLACEMENT_3D ( 'NONE', #2355, #2625, #2312 ) ;
#3810 = FACE_OUTER_BOUND ( 'NONE', #3494, .T. ) ;
#3811 = CIRCLE ( 'NONE', #4414, 3.573749999999998650 ) ;
#3812 = CYLINDRICAL_SURFACE ( 'NONE', #1118, 3.573749999999999538 ) ;
#3813 = ORIENTED_EDGE ( 'NONE', *, *, #1354, .T. ) ;
#3814 = ORIENTED_EDGE ( 'NONE', *, *, #4429, .T. ) ;
#3815 = VECTOR ( 'NONE', #3621, 1000.000000000000000 ) ;
#3816 = CARTESIAN_POINT ( 'NONE',  ( -7.619992765438045268, 0.004097986548673348585, 31.86762445358909446 ) ) ;
#3817 = ORIENTED_EDGE ( 'NONE', *, *, #2751, .F. ) ;
#3818 = CARTESIAN_POINT ( 'NONE',  ( -3.749999999999999556, -3.750000000000000888, 146.2500000000000000 ) ) ;
#3819 = CARTESIAN_POINT ( 'NONE',  ( -8.423108025121083031, 1.344458927240798740, 56.18096039353566340 ) ) ;
#3820 = ADVANCED_FACE ( 'NONE', ( #1611 ), #2342, .T. ) ;
#3821 = CARTESIAN_POINT ( 'NONE',  ( -14.28160183601729472, -0.4706309645614943360, 35.91635743244306411 ) ) ;
#3822 = DIRECTION ( 'NONE',  ( 0.000000000000000000, 0.000000000000000000, 1.000000000000000000 ) ) ;
#3823 = SURFACE_SIDE_STYLE ('',( #4556 ) ) ;
#3824 = DIRECTION ( 'NONE',  ( 8.673617379884035472E-17, 1.000000000000000000, 0.000000000000000000 ) ) ;
#3825 = AXIS2_PLACEMENT_3D ( 'NONE', #3070, #1203, #1602 ) ;
#3826 = CARTESIAN_POINT ( 'NONE',  ( 2.316727177394500794E-17, 0.000000000000000000, 1.587499999999999467 ) ) ;
#3827 = ORIENTED_EDGE ( 'NONE', *, *, #2174, .F. ) ;
#3828 = CARTESIAN_POINT ( 'NONE',  ( -14.28750000000000142, -3.249382362871961689E-18, 18.74999999999999645 ) ) ;
#3829 = ORIENTED_EDGE ( 'NONE', *, *, #1376, .T. ) ;
#3830 = CARTESIAN_POINT ( 'NONE',  ( 12.58716276799420797, -6.756261061128872036, 34.20002532364929237 ) ) ;
#3831 = CARTESIAN_POINT ( 'NONE',  ( -12.37116490068861197, -7.143402013451321864, 17.15262445358908039 ) ) ;
#3832 = ORIENTED_EDGE ( 'NONE', *, *, #1769, .T. ) ;
#3833 =( REPRESENTATION_RELATIONSHIP ('NONE','NONE', #4401, #3415 ) REPRESENTATION_RELATIONSHIP_WITH_TRANSFORMATION ( #804 )SHAPE_REPRESENTATION_RELATIONSHIP( ) );
#3834 = ORIENTED_EDGE ( 'NONE', *, *, #734, .F. ) ;
#3835 = EDGE_CURVE ( 'NONE', #3411, #4497, #922, .T. ) ;
#3836 = AXIS2_PLACEMENT_3D ( 'NONE', #3894, #2738, #1343 ) ;
#3837 = DIRECTION ( 'NONE',  ( 0.000000000000000000, 0.000000000000000000, 1.000000000000000000 ) ) ;
#3838 = AXIS2_PLACEMENT_3D ( 'NONE', #3356, #2997, #4465 ) ;
#3839 = ADVANCED_FACE ( 'NONE', ( #3810 ), #2318, .T. ) ;
#3840 = ORIENTED_EDGE ( 'NONE', *, *, #158, .F. ) ;
#3841 = LINE ( 'NONE', #3516, #2028 ) ;
#3842 = AXIS2_PLACEMENT_3D ( 'NONE', #898, #4383, #4022 ) ;
#3843 = CARTESIAN_POINT ( 'NONE',  ( -14.26328418769022122, -0.9536332803280443970, 39.46541283322252980 ) ) ;
#3844 = CARTESIAN_POINT ( 'NONE',  ( 14.17128811577592451, -1.877060880510151852, 39.27869980365568381 ) ) ;
#3845 = CARTESIAN_POINT ( 'NONE',  ( 13.83333314027810346, -3.573749167952787964, 32.60299647559080682 ) ) ;
#3846 = CARTESIAN_POINT ( 'NONE',  ( 13.73375050552179744, -10.16000000000000014, 6.586250505521794807 ) ) ;
#3847 = DIRECTION ( 'NONE',  ( 1.000000000000000000, 0.000000000000000000, 0.000000000000000000 ) ) ;
#3848 = CARTESIAN_POINT ( 'NONE',  ( -8.369994990996019624, -6.397499167952786614, 32.36596039353565857 ) ) ;
#3849 = VECTOR ( 'NONE', #3513, 1000.000000000000000 ) ;
#3850 = VERTEX_POINT ( 'NONE', #4142 ) ;
#3851 = ADVANCED_FACE ( 'NONE', ( #4500 ), #2239, .T. ) ;
#3852 = FACE_OUTER_BOUND ( 'NONE', #405, .T. ) ;
#3853 = CARTESIAN_POINT ( 'NONE',  ( 18.74250500900397753, 8.320472107924325483E-07, 32.36596039353566567 ) ) ;
#3854 = ADVANCED_FACE ( 'NONE', ( #1261, #564 ), #897, .F. ) ;
#3855 = ORIENTED_EDGE ( 'NONE', *, *, #2529, .F. ) ;
#3856 = ORIENTED_EDGE ( 'NONE', *, *, #166, .F. ) ;
#3857 = EDGE_CURVE ( 'NONE', #2299, #2304, #436, .T. ) ;
#3858 = SURFACE_STYLE_FILL_AREA ( #4596 ) ;
#3859 = EDGE_LOOP ( 'NONE', ( #3730, #91, #277, #1967, #2674 ) ) ;
#3860 = CARTESIAN_POINT ( 'NONE',  ( 13.73375050552179744, -10.16000000000000014, 17.78000050552179445 ) ) ;
#3861 = CYLINDRICAL_SURFACE ( 'NONE', #4043, 0.7500000000000006661 ) ;
#3862 = CARTESIAN_POINT ( 'NONE',  ( -14.25898756740889439, -0.9310840564244263762, 35.82426841225251479 ) ) ;
#3863 = CARTESIAN_POINT ( 'NONE',  ( 13.11669703816544619, -5.666583100918747284, 36.72824904517413103 ) ) ;
#3864 = DIRECTION ( 'NONE',  ( -0.000000000000000000, -0.000000000000000000, -1.000000000000000000 ) ) ;
#3865 =( GEOMETRIC_REPRESENTATION_CONTEXT ( 3 ) GLOBAL_UNCERTAINTY_ASSIGNED_CONTEXT ( ( #4485 ) ) GLOBAL_UNIT_ASSIGNED_CONTEXT ( ( #1364, #2018, #4243 ) ) REPRESENTATION_CONTEXT ( 'NONE', 'WORKASPACE' ) );
#3866 = EDGE_CURVE ( 'NONE', #2091, #4049, #2675, .T. ) ;
#3867 = CARTESIAN_POINT ( 'NONE',  ( -14.03274124047852744, -2.687123044775775238, 29.50471817954215581 ) ) ;
#3868 = DIRECTION ( 'NONE',  ( -0.000000000000000000, -0.000000000000000000, -1.000000000000000000 ) ) ;
#3869 = DIRECTION ( 'NONE',  ( 1.000000000000000000, 0.000000000000000000, -0.000000000000000000 ) ) ;
#3870 = AXIS2_PLACEMENT_3D ( 'NONE', #1543, #1522, #2935 ) ;
#3871 = LINE ( 'NONE', #3897, #1968 ) ;
#3872 = ORIENTED_EDGE ( 'NONE', *, *, #1934, .F. ) ;
#3873 = CARTESIAN_POINT ( 'NONE',  ( 8.370007234561949616, 6.401597986548672736, 17.90262445358908039 ) ) ;
#3874 = ADVANCED_FACE ( 'NONE', ( #4006 ), #2217, .T. ) ;
#3875 = AXIS2_PLACEMENT_3D ( 'NONE', #4218, #636, #4240 ) ;
#3876 = PRODUCT ( 'Part 133_Varsay\X2\0131\X0\lan', 'Part 133_Varsay\X2\0131\X0\lan', '', ( #778 ) ) ;
#3877 = EDGE_CURVE ( 'NONE', #3060, #3850, #3056, .T. ) ;
#3878 = CARTESIAN_POINT ( 'NONE',  ( 12.37117714425454551, -7.147499167952784838, 18.40096039353565160 ) ) ;
#3879 = DIRECTION ( 'NONE',  ( 9.517981353260378315E-33, -8.841607930564763213E-17, 1.000000000000000000 ) ) ;
#3880 = AXIS2_PLACEMENT_3D ( 'NONE', #2434, #587, #2009 ) ;
#3881 = ORIENTED_EDGE ( 'NONE', *, *, #3448, .T. ) ;
#3882 = ORIENTED_EDGE ( 'NONE', *, *, #2192, .F. ) ;
#3883 = EDGE_CURVE ( 'NONE', #356, #21, #732, .T. ) ;
#3884 = CARTESIAN_POINT ( 'NONE',  ( 5.009003980371977336E-06, 8.320472128100606877E-07, 17.65096039353565160 ) ) ;
#3885 = ORIENTED_EDGE ( 'NONE', *, *, #2190, .T. ) ;
#3886 = DIRECTION ( 'NONE',  ( 0.000000000000000000, 0.000000000000000000, 1.000000000000000000 ) ) ;
#3887 = VERTEX_POINT ( 'NONE', #1664 ) ;
#3888 = CARTESIAN_POINT ( 'NONE',  ( 17.28000050552179445, -3.039999999999999591, 17.78000050552179445 ) ) ;
#3889 = CARTESIAN_POINT ( 'NONE',  ( -12.37116712624658810, -7.147499167952786614, 32.84697568125972822 ) ) ;
#3890 = CARTESIAN_POINT ( 'NONE',  ( 2.540000505521796015, -17.28000000000000114, 3.040000505521795571 ) ) ;
#3891 = FILL_AREA_STYLE ('',( #3521 ) ) ;
#3892 = VECTOR ( 'NONE', #1363, 1000.000000000000000 ) ;
#3893 = CARTESIAN_POINT ( 'NONE',  ( 17.28000050552179800, -17.28000000000000114, 2.540000505521796015 ) ) ;
#3894 = CARTESIAN_POINT ( 'NONE',  ( 3.040000505521796015, -3.039999999999999591, 17.28000050552179445 ) ) ;
#3895 = DIRECTION ( 'NONE',  ( 0.000000000000000000, 0.000000000000000000, 1.000000000000000000 ) ) ;
#3896 = CARTESIAN_POINT ( 'NONE',  ( 7.620007234561951392, 12.08996809382683857, 17.90262445358908039 ) ) ;
#3897 = CARTESIAN_POINT ( 'NONE',  ( 17.78000050552179445, -10.16000000000000014, 6.586250505521796583 ) ) ;
#3898 = AXIS2_PLACEMENT_3D ( 'NONE', #3726, #4085, #1298 ) ;
#3899 = ORIENTED_EDGE ( 'NONE', *, *, #2273, .F. ) ;
#3900 = DIRECTION ( 'NONE',  ( 1.000000000000000000, -1.076498916035107621E-16, -0.000000000000000000 ) ) ;
#3901 = FACE_OUTER_BOUND ( 'NONE', #903, .T. ) ;
#3902 = EDGE_CURVE ( 'NONE', #245, #3774, #1175, .T. ) ;
#3903 = VERTEX_POINT ( 'NONE', #2365 ) ;
#3904 = EDGE_LOOP ( 'NONE', ( #3038, #3420, #4432, #3136 ) ) ;
#3905 = AXIS2_PLACEMENT_3D ( 'NONE', #4555, #4221, #1001 ) ;
#3906 = EDGE_CURVE ( 'NONE', #3059, #1488, #2780, .T. ) ;
#3907 = VERTEX_POINT ( 'NONE', #654 ) ;
#3908 = DIRECTION ( 'NONE',  ( 1.000000000000000000, 0.000000000000000000, 0.000000000000000000 ) ) ;
#3909 = CARTESIAN_POINT ( 'NONE',  ( -14.28749276543805102, 0.2378296109429726690, 28.29387445358910469 ) ) ;
#3910 = APPLICATION_PROTOCOL_DEFINITION ( 'draft international standard', 'automotive_design', 1998, #2244 ) ;
#3911 = VECTOR ( 'NONE', #3282, 1000.000000000000000 ) ;
#3912 = VECTOR ( 'NONE', #2765, 1000.000000000000000 ) ;
#3913 = DIRECTION ( 'NONE',  ( -0.000000000000000000, -0.000000000000000000, -1.000000000000000000 ) ) ;
#3914 = CARTESIAN_POINT ( 'NONE',  ( 14.26331392418316213, -0.9521779091557251995, 39.46544505580351370 ) ) ;
#3915 = CIRCLE ( 'NONE', #1150, 1.499999999999999556 ) ;
#3916 = DIRECTION ( 'NONE',  ( -8.673617379884035472E-17, 1.000000000000000000, -0.000000000000000000 ) ) ;
#3917 = CARTESIAN_POINT ( 'NONE',  ( -14.24246651021981336, 1.153954063360001614, 28.97559098912187991 ) ) ;
#3918 = DIRECTION ( 'NONE',  ( -0.000000000000000000, -0.000000000000000000, -1.000000000000000000 ) ) ;
#3919 = LINE ( 'NONE', #3505, #1368 ) ;
#3920 = DIRECTION ( 'NONE',  ( -0.000000000000000000, -0.000000000000000000, -1.000000000000000000 ) ) ;
#3921 = TOROIDAL_SURFACE ( 'NONE', #1074, 6.397499999999999964, 0.7500000000000000000 ) ;
#3922 = ORIENTED_EDGE ( 'NONE', *, *, #3175, .F. ) ;
#3923 = CARTESIAN_POINT ( 'NONE',  ( -7.619994990996019624, 8.320472136303528048E-07, 32.36596039353566567 ) ) ;
#3924 =( REPRESENTATION_RELATIONSHIP ('NONE','NONE', #4401, #1005 ) REPRESENTATION_RELATIONSHIP_WITH_TRANSFORMATION ( #4433 )SHAPE_REPRESENTATION_RELATIONSHIP( ) );
#3925 = DIRECTION ( 'NONE',  ( 1.000000000000000000, 0.000000000000000000, 0.000000000000000000 ) ) ;
#3926 = ORIENTED_EDGE ( 'NONE', *, *, #233, .T. ) ;
#3927 = B_SPLINE_CURVE_WITH_KNOTS ( 'NONE', 3,
 ( #4079, #3675, #148, #1919, #102, #4124, #3373, #453, #1945, #2616 ),
 .UNSPECIFIED., .F., .F.,
 ( 4, 2, 2, 2, 4 ),
 ( 0.000000000000000000, 0.0003186827706029869483, 0.0006373655412059738967, 0.0009560483118089608450, 0.001274731082411947793 ),
 .UNSPECIFIED. ) ;
#3928 = ORIENTED_EDGE ( 'NONE', *, *, #3175, .T. ) ;
#3929 = EDGE_CURVE ( 'NONE', #2486, #2613, #3968, .T. ) ;
#3930 = CARTESIAN_POINT ( 'NONE',  ( -13.05553636216897573, 5.809745059568978576, 36.04312068514321510 ) ) ;
#3931 = AXIS2_PLACEMENT_3D ( 'NONE', #400, #1402, #3925 ) ;
#3932 = ORIENTED_EDGE ( 'NONE', *, *, #2676, .F. ) ;
#3933 = FACE_OUTER_BOUND ( 'NONE', #3111, .T. ) ;
#3934 = DIRECTION ( 'NONE',  ( -1.000000000000000000, 1.076498916035107744E-16, 0.000000000000000000 ) ) ;
#3935 =( LENGTH_UNIT ( ) NAMED_UNIT ( * ) SI_UNIT ( .MILLI., .METRE. ) );
#3936 = EDGE_CURVE ( 'NONE', #3411, #1208, #162, .T. ) ;
#3937 = EDGE_CURVE ( 'NONE', #3784, #195, #304, .T. ) ;
#3938 = CARTESIAN_POINT ( 'NONE',  ( -1.395705466780353232, -3.565902013451327512, -9.479113238741371461 ) ) ;
#3939 = CARTESIAN_POINT ( 'NONE',  ( -14.28749499099602005, 8.320472128100571937E-07, 28.79221039353566880 ) ) ;
#3940 = EDGE_CURVE ( 'NONE', #1513, #4636, #1401, .T. ) ;
#3941 = FACE_OUTER_BOUND ( 'NONE', #3347, .T. ) ;
#3942 = CARTESIAN_POINT ( 'NONE',  ( -8.369992765438045268, -6.393402013451324528, 17.90262445358908039 ) ) ;
#3943 = DIRECTION ( 'NONE',  ( 0.000000000000000000, -1.000000000000000000, 0.000000000000000000 ) ) ;
#3944 = EDGE_CURVE ( 'NONE', #1617, #230, #2767, .T. ) ;
#3945 = EDGE_CURVE ( 'NONE', #2464, #2260, #2453, .T. ) ;
#3946 = VERTEX_POINT ( 'NONE', #1775 ) ;
#3947 = CARTESIAN_POINT ( 'NONE',  ( 14.20052877066713037, 1.589184853276433662, 35.57557690958116581 ) ) ;
#3948 = CARTESIAN_POINT ( 'NONE',  ( -13.48443111421813256, -4.722189432810507626, 37.23438744284855773 ) ) ;
#3949 = CARTESIAN_POINT ( 'NONE',  ( 18.74250500900397753, 8.320472107924325483E-07, 32.36596039353566567 ) ) ;
#3950 = VECTOR ( 'NONE', #3868, 1000.000000000000000 ) ;
#3951 = ORIENTED_EDGE ( 'NONE', *, *, #4005, .T. ) ;
#3952 = VERTEX_POINT ( 'NONE', #3199 ) ;
#3953 =( LENGTH_UNIT ( ) NAMED_UNIT ( * ) SI_UNIT ( .MILLI., .METRE. ) );
#3954 = VERTEX_POINT ( 'NONE', #1423 ) ;
#3955 = ORIENTED_EDGE ( 'NONE', *, *, #1449, .F. ) ;
#3956 = B_SPLINE_CURVE_WITH_KNOTS ( 'NONE', 3,
 ( #731, #2916, #428, #779, #1872, #4506, #1219, #3036, #2988, #2614, #3400, #1593, #174, #4457, #497, #4481, #550, #1197 ),
 .UNSPECIFIED., .F., .F.,
 ( 4, 2, 2, 2, 2, 2, 2, 2, 4 ),
 ( 0.005610345619348811042, 0.006311274135232912939, 0.007012202651117014837, 0.007713131167001116735, 0.008414059682885218633, 0.009114988198769319663, 0.009815916714653420694, 0.01051684523053752346, 0.01121777374642162449 ),
 .UNSPECIFIED. ) ;
#3957 = DIRECTION ( 'NONE',  ( -0.000000000000000000, -0.000000000000000000, -1.000000000000000000 ) ) ;
#3958 = AXIS2_PLACEMENT_3D ( 'NONE', #612, #4568, #3058 ) ;
#3959 = CARTESIAN_POINT ( 'NONE',  ( -8.423113034125059073, 3.330709759288002392, -81.10307921292867661 ) ) ;
#3960 = CARTESIAN_POINT ( 'NONE',  ( 8.370005009003978813, 7.147500832047211539, 18.40096039353565160 ) ) ;
#3961 = CARTESIAN_POINT ( 'NONE',  ( -1.123311860454918376, -3.565902013451327068, -9.572186130557330586 ) ) ;
#3962 = LINE ( 'NONE', #1768, #1767 ) ;
#3963 = CARTESIAN_POINT ( 'NONE',  ( -13.83332312227014427, 3.573750832047213777, 32.36596039353566567 ) ) ;
#3964 = CARTESIAN_POINT ( 'NONE',  ( -14.28749499099602005, 8.320472128100606877E-07, 3.790960393535649064 ) ) ;
#3965 = VECTOR ( 'NONE', #4226, 1000.000000000000000 ) ;
#3966 = FACE_OUTER_BOUND ( 'NONE', #2913, .T. ) ;
#3967 = CARTESIAN_POINT ( 'NONE',  ( 14.17614002078996727, -1.787162261592786683, 34.96891191078774597 ) ) ;
#3968 = CIRCLE ( 'NONE', #216, 4.762499999999999289 ) ;
#3969 = CARTESIAN_POINT ( 'NONE',  ( 12.13299322807326064, -7.545448496333294841, 17.73224578507567628 ) ) ;
#3970 = ADVANCED_BREP_SHAPE_REPRESENTATION ( '', ( #275, #4483 ), #4552 ) ;
#3971 = ORIENTED_EDGE ( 'NONE', *, *, #263, .T. ) ;
#3972 = CARTESIAN_POINT ( 'NONE',  ( -3.749999999999999556, -3.750000000000000888, 146.2500000000000000 ) ) ;
#3973 = DIRECTION ( 'NONE',  ( 0.000000000000000000, 0.000000000000000000, 1.000000000000000000 ) ) ;
#3974 = FACE_OUTER_BOUND ( 'NONE', #982, .T. ) ;
#3975 = ORIENTED_EDGE ( 'NONE', *, *, #846, .F. ) ;
#3976 = AXIS2_PLACEMENT_3D ( 'NONE', #4170, #1121, #1092 ) ;
#3977 = ORIENTED_EDGE ( 'NONE', *, *, #993, .T. ) ;
#3978 = B_SPLINE_CURVE_WITH_KNOTS ( 'NONE', 3,
 ( #1913, #4070, #1443, #3263, #709, #58, #3610, #1460, #2173, #1502, #2570, #1100, #340, #2148, #1829, #1049, #2850, #4010, #780, #759, #4294, #2517, #2198, #3632 ),
 .UNSPECIFIED., .F., .F.,
 ( 4, 2, 2, 2, 2, 2, 2, 2, 2, 2, 2, 4 ),
 ( 0.000000000000000000, 0.001420218485702549145, 0.002840436971405098290, 0.004260655457107647218, 0.004970764699958913659, 0.005680873942810180099, 0.006390983185661445673, 0.007101092428512711247, 0.008521310914215231985, 0.009231420157066490620, 0.009941529399917750989, 0.01136174788562027173 ),
 .UNSPECIFIED. ) ;
#3979 = ORIENTED_EDGE ( 'NONE', *, *, #4196, .T. ) ;
#3980 = EDGE_CURVE ( 'NONE', #1822, #421, #2302, .T. ) ;
#3981 = PRODUCT_DEFINITION ( 'UNKNOWN', '', #787, #3006 ) ;
#3982 = EDGE_CURVE ( 'NONE', #1713, #1450, #3061, .T. ) ;
#3983 = AXIS2_PLACEMENT_3D ( 'NONE', #1721, #4227, #2089 ) ;
#3984 = CARTESIAN_POINT ( 'NONE',  ( 7.234561953626996335E-06, 0.004097986548672528061, 17.15262445358908039 ) ) ;
#3985 = ADVANCED_FACE ( 'NONE', ( #4232 ), #2743, .F. ) ;
#3986 = CARTESIAN_POINT ( 'NONE',  ( -27.47310802512107841, 3.330708927240775719, -113.4690396064643636 ) ) ;
#3987 = FACE_OUTER_BOUND ( 'NONE', #1288, .T. ) ;
#3988 = CARTESIAN_POINT ( 'NONE',  ( 6.870007234561953169, 0.004097986548673267920, 17.15262445358908039 ) ) ;
#3989 = APPLICATION_CONTEXT ( 'automotive_design' ) ;
#3990 = FACE_OUTER_BOUND ( 'NONE', #1314, .T. ) ;
#3991 = CARTESIAN_POINT ( 'NONE',  ( 14.28750723456195537, 0.004097986548674278397, 39.01512445358908820 ) ) ;
#3992 = VECTOR ( 'NONE', #1463, 1000.000000000000000 ) ;
#3993 = CARTESIAN_POINT ( 'NONE',  ( 14.28750000000000142, 1.746464731918909201E-15, 131.2499999999999716 ) ) ;
#3994 = DIRECTION ( 'NONE',  ( -0.000000000000000000, -0.000000000000000000, 1.000000000000000000 ) ) ;
#3995 = ORIENTED_EDGE ( 'NONE', *, *, #3033, .F. ) ;
#3996 = CARTESIAN_POINT ( 'NONE',  ( 14.28750500900398279, 8.320472145953950175E-07, 35.93971039353566965 ) ) ;
#3997 = CARTESIAN_POINT ( 'NONE',  ( -13.30104646604472407, -5.215534672250015547, 36.75583910459432957 ) ) ;
#3998 = DIRECTION ( 'NONE',  ( -1.000000000000000000, 1.076498916035107744E-16, 0.000000000000000000 ) ) ;
#3999 = EDGE_CURVE ( 'NONE', #3808, #3059, #258, .T. ) ;
#4000 = ORIENTED_EDGE ( 'NONE', *, *, #3155, .T. ) ;
#4001 = ORIENTED_EDGE ( 'NONE', *, *, #4074, .F. ) ;
#4002 =( NAMED_UNIT ( * ) SI_UNIT ( $, .STERADIAN. ) SOLID_ANGLE_UNIT ( ) );
#4003 = ADVANCED_FACE ( 'NONE', ( #3852 ), #4571, .F. ) ;
#4004 = VERTEX_POINT ( 'NONE', #2430 ) ;
#4005 = EDGE_CURVE ( 'NONE', #3671, #1779, #1186, .T. ) ;
#4006 = FACE_OUTER_BOUND ( 'NONE', #937, .T. ) ;
#4007 = APPLICATION_PROTOCOL_DEFINITION ( 'draft international standard', 'automotive_design', 1998, #4320 ) ;
#4008 = DIRECTION ( 'NONE',  ( -1.000000000000000000, 1.076498916035107744E-16, -0.000000000000000000 ) ) ;
#4009 = VECTOR ( 'NONE', #1473, 1000.000000000000000 ) ;
#4010 = CARTESIAN_POINT ( 'NONE',  ( 14.05881308173377775, 2.559578388020689488, 38.54673083970038761 ) ) ;
#4011 = CARTESIAN_POINT ( 'NONE',  ( 2.316727177394501718E-17, 0.000000000000000000, 4.762500000000001066 ) ) ;
#4012 = CARTESIAN_POINT ( 'NONE',  ( 7.620007234561954057, -6.393402013451328081, 31.86762445358908735 ) ) ;
#4013 = DIRECTION ( 'NONE',  ( 0.000000000000000000, 0.000000000000000000, 1.000000000000000000 ) ) ;
#4014 = CARTESIAN_POINT ( 'NONE',  ( -14.17582073965153278, -1.789560200172800153, 34.96752390565762880 ) ) ;
#4015 = DIRECTION ( 'NONE',  ( 0.000000000000000000, -1.000000000000000000, 0.000000000000000000 ) ) ;
#4016 = ORIENTED_EDGE ( 'NONE', *, *, #792, .F. ) ;
#4017 = CARTESIAN_POINT ( 'NONE',  ( 13.83333314027810701, 3.573750832047210668, 32.36596039353566567 ) ) ;
#4018 = DIRECTION ( 'NONE',  ( 0.000000000000000000, 1.000000000000000000, -0.000000000000000000 ) ) ;
#4019 = ORIENTED_EDGE ( 'NONE', *, *, #114, .F. ) ;
#4020 = DIRECTION ( 'NONE',  ( 0.000000000000000000, 0.000000000000000000, 1.000000000000000000 ) ) ;
#4021 =( GEOMETRIC_REPRESENTATION_CONTEXT ( 3 ) GLOBAL_UNCERTAINTY_ASSIGNED_CONTEXT ( ( #3449 ) ) GLOBAL_UNIT_ASSIGNED_CONTEXT ( ( #2993, #4438, #1574 ) ) REPRESENTATION_CONTEXT ( 'NONE', 'WORKASPACE' ) );
#4022 = DIRECTION ( 'NONE',  ( 0.000000000000000000, -1.000000000000000000, 0.000000000000000000 ) ) ;
#4023 = EDGE_CURVE ( 'NONE', #195, #4203, #888, .T. ) ;
#4024 = DIRECTION ( 'NONE',  ( 0.000000000000000000, 0.000000000000000000, 1.000000000000000000 ) ) ;
#4025 = VECTOR ( 'NONE', #1505, 1000.000000000000000 ) ;
#4026 = ORIENTED_EDGE ( 'NONE', *, *, #2098, .T. ) ;
#4027 = EDGE_LOOP ( 'NONE', ( #2886, #3673, #653, #3158 ) ) ;
#4028 = CARTESIAN_POINT ( 'NONE',  ( -14.12134855583884629, 2.181372335837979737, 35.20634009499998029 ) ) ;
#4029 = VECTOR ( 'NONE', #825, 1000.000000000000000 ) ;
#4030 = DIRECTION ( 'NONE',  ( 0.000000000000000000, 0.000000000000000000, -1.000000000000000000 ) ) ;
#4031 = ORIENTED_EDGE ( 'NONE', *, *, #3256, .F. ) ;
#4032 = AXIS2_PLACEMENT_3D ( 'NONE', #4592, #239, #4189 ) ;
#4033 = SURFACE_STYLE_USAGE ( .BOTH. , #1900 ) ;
#4034 = AXIS2_PLACEMENT_3D ( 'NONE', #3816, #4150, #4507 ) ;
#4035 =( LENGTH_UNIT ( ) NAMED_UNIT ( * ) SI_UNIT ( .MILLI., .METRE. ) );
#4036 = DIRECTION ( 'NONE',  ( 8.673617379884035472E-17, 1.000000000000000000, -0.000000000000000000 ) ) ;
#4037 = CARTESIAN_POINT ( 'NONE',  ( -13.83332089671217346, -3.569652013451324990, 32.10328778829815377 ) ) ;
#4038 = CARTESIAN_POINT ( 'NONE',  ( 12.37117714425454551, -7.147499167952784838, 18.40096039353565160 ) ) ;
#4039 = AXIS2_PLACEMENT_3D ( 'NONE', #466, #4421, #838 ) ;
#4040 = VERTEX_POINT ( 'NONE', #3313 ) ;
#4041 = FACE_OUTER_BOUND ( 'NONE', #3511, .T. ) ;
#4042 = CARTESIAN_POINT ( 'NONE',  ( -9.549434556529077899E-17, -3.249382362871961689E-18, 18.74999999999999645 ) ) ;
#4043 = AXIS2_PLACEMENT_3D ( 'NONE', #999, #3427, #4129 ) ;
#4044 = ORIENTED_EDGE ( 'NONE', *, *, #3677, .T. ) ;
#4045 = CARTESIAN_POINT ( 'NONE',  ( 17.28000050552179445, -3.039999999999999591, 3.040000505521795571 ) ) ;
#4046 = DIRECTION ( 'NONE',  ( -0.000000000000000000, -0.000000000000000000, -1.000000000000000000 ) ) ;
#4047 = DIRECTION ( 'NONE',  ( -1.000000000000000000, 8.673617379884026597E-16, 0.000000000000000000 ) ) ;
#4048 = CARTESIAN_POINT ( 'NONE',  ( 6.586250505521797471, -10.16000000000000014, 13.73375050552179744 ) ) ;
#4049 = VERTEX_POINT ( 'NONE', #1539 ) ;
#4050 = CIRCLE ( 'NONE', #3898, 0.7500000000000006661 ) ;
#4051 = EDGE_LOOP ( 'NONE', ( #1659, #2938, #3881, #172, #4377 ) ) ;
#4052 = CONTEXT_DEPENDENT_SHAPE_REPRESENTATION ( #3684, #1994 ) ;
#4053 = CARTESIAN_POINT ( 'NONE',  ( 18.74250723456195189, -3.569652013451328987, 31.86762445358909446 ) ) ;
#4054 = ADVANCED_FACE ( 'NONE', ( #2952 ), #2208, .F. ) ;
#4055 = CARTESIAN_POINT ( 'NONE',  ( 10.16000050552179701, -10.16000000000000014, 17.78000050552179445 ) ) ;
#4056 = ORIENTED_EDGE ( 'NONE', *, *, #2080, .T. ) ;
#4057 = CARTESIAN_POINT ( 'NONE',  ( 14.99250500900398109, 7.147500832047209762, 32.36596039353565857 ) ) ;
#4058 = CARTESIAN_POINT ( 'NONE',  ( 3.573757234561953045, 0.004097986548672966078, 17.16762445358907385 ) ) ;
#4059 = CARTESIAN_POINT ( 'NONE',  ( -13.83332089671217169, 3.577847986548673642, 31.86762445358909446 ) ) ;
#4060 = DIRECTION ( 'NONE',  ( 1.000000000000000000, 0.000000000000000000, 0.000000000000000000 ) ) ;
#4061 = DIRECTION ( 'NONE',  ( 1.000000000000000000, -1.076498916035107621E-16, -0.000000000000000000 ) ) ;
#4062 = ORIENTED_EDGE ( 'NONE', *, *, #600, .F. ) ;
#4063 = FACE_OUTER_BOUND ( 'NONE', #4286, .T. ) ;
#4064 =( GEOMETRIC_REPRESENTATION_CONTEXT ( 3 ) GLOBAL_UNCERTAINTY_ASSIGNED_CONTEXT ( ( #2348 ) ) GLOBAL_UNIT_ASSIGNED_CONTEXT ( ( #740, #1838, #42 ) ) REPRESENTATION_CONTEXT ( 'NONE', 'WORKASPACE' ) );
#4065 = DIRECTION ( 'NONE',  ( -9.517981353260378315E-33, 8.841607930564763213E-17, -1.000000000000000000 ) ) ;
#4066 = DIRECTION ( 'NONE',  ( -1.000000000000000000, 0.000000000000000000, 0.000000000000000000 ) ) ;
#4067 = VERTEX_POINT ( 'NONE', #2555 ) ;
#4068 = DIRECTION ( 'NONE',  ( 1.000000000000000000, 0.000000000000000000, 0.000000000000000000 ) ) ;
#4069 = VECTOR ( 'NONE', #827, 1000.000000000000000 ) ;
#4070 = CARTESIAN_POINT ( 'NONE',  ( 12.37117936981251809, 7.151597986548668295, 32.34863974131316411 ) ) ;
#4071 = DIRECTION ( 'NONE',  ( 0.000000000000000000, 0.000000000000000000, -1.000000000000000000 ) ) ;
#4072 = AXIS2_PLACEMENT_3D ( 'NONE', #4447, #2293, #4113 ) ;
#4073 = DIRECTION ( 'NONE',  ( -1.355782318074878530E-16, 1.000000000000000000, 0.000000000000000000 ) ) ;
#4074 = EDGE_CURVE ( 'NONE', #2770, #3535, #1116, .T. ) ;
#4075 = ORIENTED_EDGE ( 'NONE', *, *, #1792, .F. ) ;
#4076 = ORIENTED_EDGE ( 'NONE', *, *, #2471, .F. ) ;
#4077 = CONTEXT_DEPENDENT_SHAPE_REPRESENTATION ( #2072, #2733 ) ;
#4078 = LINE ( 'NONE', #4408, #645 ) ;
#4079 = CARTESIAN_POINT ( 'NONE',  ( -11.90638390633376709, -7.893402013451320975, 17.15262445358908039 ) ) ;
#4080 =( GEOMETRIC_REPRESENTATION_CONTEXT ( 3 ) GLOBAL_UNCERTAINTY_ASSIGNED_CONTEXT ( ( #199 ) ) GLOBAL_UNIT_ASSIGNED_CONTEXT ( ( #312, #2059, #1017 ) ) REPRESENTATION_CONTEXT ( 'NONE', 'WORKASPACE' ) );
#4081 = ORIENTED_EDGE ( 'NONE', *, *, #951, .T. ) ;
#4082 = EDGE_CURVE ( 'NONE', #657, #728, #431, .T. ) ;
#4083 = CARTESIAN_POINT ( 'NONE',  ( 8.066546224052645542, -6.586249999999999716, 8.066546224052645542 ) ) ;
#4084 = EDGE_CURVE ( 'NONE', #3180, #4067, #3446, .T. ) ;
#4085 = DIRECTION ( 'NONE',  ( 0.000000000000000000, -0.000000000000000000, 1.000000000000000000 ) ) ;
#4086 = DIRECTION ( 'NONE',  ( 0.000000000000000000, 0.000000000000000000, -1.000000000000000000 ) ) ;
#4087 = DIRECTION ( 'NONE',  ( 0.000000000000000000, 0.000000000000000000, 1.000000000000000000 ) ) ;
#4088 = AXIS2_PLACEMENT_3D ( 'NONE', #3214, #1101, #3264 ) ;
#4089 = ADVANCED_FACE ( 'NONE', ( #3640, #2904 ), #4350, .T. ) ;
#4090 = VERTEX_POINT ( 'NONE', #1514 ) ;
#4091 = EDGE_CURVE ( 'NONE', #680, #4479, #767, .T. ) ;
#4092 = CARTESIAN_POINT ( 'NONE',  ( 18.74250500900397753, 8.320472107924325483E-07, 32.36596039353566567 ) ) ;
#4093 = CARTESIAN_POINT ( 'NONE',  ( 14.20066920646721620, 1.591968333033273231, 28.65740429563327396 ) ) ;
#4094 = FACE_OUTER_BOUND ( 'NONE', #3710, .T. ) ;
#4095 = VERTEX_POINT ( 'NONE', #3246 ) ;
#4096 = FACE_OUTER_BOUND ( 'NONE', #2607, .T. ) ;
#4097 = CARTESIAN_POINT ( 'NONE',  ( 3.040000505521796015, -3.039999999999999591, 2.540000505521796015 ) ) ;
#4098 = CARTESIAN_POINT ( 'NONE',  ( -3.750000000000000888, -3.750000000000000000, 3.749999999999995559 ) ) ;
#4099 = ORIENTED_EDGE ( 'NONE', *, *, #4428, .T. ) ;
#4100 = ORIENTED_EDGE ( 'NONE', *, *, #1793, .F. ) ;
#4101 = FACE_OUTER_BOUND ( 'NONE', #1384, .T. ) ;
#4102 = CARTESIAN_POINT ( 'NONE',  ( 2.316727177394501718E-17, 0.000000000000000000, 33.33750000000000568 ) ) ;
#4103 = ORIENTED_EDGE ( 'NONE', *, *, #3424, .T. ) ;
#4104 = PLANE ( 'NONE',  #683 ) ;
#4105 = AXIS2_PLACEMENT_3D ( 'NONE', #3372, #2964, #878 ) ;
#4106 = LINE ( 'NONE', #1901, #1810 ) ;
#4107 = CARTESIAN_POINT ( 'NONE',  ( 13.42356276806338400, 4.895988140896816887, 37.57830303755702062 ) ) ;
#4108 = DIRECTION ( 'NONE',  ( 0.000000000000000000, -0.000000000000000000, -1.000000000000000000 ) ) ;
#4109 = CARTESIAN_POINT ( 'NONE',  ( -3.750000000000000000, 3.750000000000000000, 3.749999999999995559 ) ) ;
#4110 = ADVANCED_FACE ( 'NONE', ( #4041, #1841 ), #1442, .F. ) ;
#4111 = ORIENTED_EDGE ( 'NONE', *, *, #3005, .T. ) ;
#4112 = LINE ( 'NONE', #512, #3217 ) ;
#4113 = DIRECTION ( 'NONE',  ( 0.000000000000000000, -1.000000000000000000, 0.000000000000000000 ) ) ;
#4114 = EDGE_CURVE ( 'NONE', #2014, #1947, #2377, .T. ) ;
#4115 = CARTESIAN_POINT ( 'NONE',  ( 7.620005009003978813, 8.320472118282937035E-07, 32.36596039353565857 ) ) ;
#4116 = EDGE_LOOP ( 'NONE', ( #3723, #1884 ) ) ;
#4117 = CARTESIAN_POINT ( 'NONE',  ( -14.24230558378153511, 1.156047234311700977, 35.75566482172504834 ) ) ;
#4118 = FACE_OUTER_BOUND ( 'NONE', #4564, .T. ) ;
#4119 = AXIS2_PLACEMENT_3D ( 'NONE', #3888, #1827, #3261 ) ;
#4120 = DIRECTION ( 'NONE',  ( -1.707404996040164265E-16, 1.000000000000000000, 0.000000000000000000 ) ) ;
#4121 = VERTEX_POINT ( 'NONE', #2138 ) ;
#4122 = ORIENTED_EDGE ( 'NONE', *, *, #4567, .T. ) ;
#4123 = DIRECTION ( 'NONE',  ( -1.000000000000000000, 0.000000000000000000, 0.000000000000000000 ) ) ;
#4124 = CARTESIAN_POINT ( 'NONE',  ( -12.27078490349716056, -7.314884922181505544, 17.41529878742304049 ) ) ;
#4125 = AXIS2_PLACEMENT_3D ( 'NONE', #2044, #1391, #2396 ) ;
#4126 = EDGE_LOOP ( 'NONE', ( #3327, #1896, #3010, #4349 ) ) ;
#4127 = EDGE_CURVE ( 'NONE', #4497, #1617, #2835, .T. ) ;
#4128 = DIRECTION ( 'NONE',  ( 0.000000000000000000, 0.000000000000000000, -1.000000000000000000 ) ) ;
#4129 = DIRECTION ( 'NONE',  ( 0.000000000000000000, -1.000000000000000000, 0.000000000000000000 ) ) ;
#4130 = AXIS2_PLACEMENT_3D ( 'NONE', #1889, #519, #2632 ) ;
#4131 = FACE_OUTER_BOUND ( 'NONE', #1972, .T. ) ;
#4132 = CARTESIAN_POINT ( 'NONE',  ( 12.39926910906711477, 7.099461186627058495, 33.31797499930307538 ) ) ;
#4133 = CARTESIAN_POINT ( 'NONE',  ( 3.040000505521796015, -17.28000000000000114, 2.540000505521796015 ) ) ;
#4134 = VERTEX_POINT ( 'NONE', #3972 ) ;
#4135 = CARTESIAN_POINT ( 'NONE',  ( 12.30738871829480807, -7.252862566945415423, 17.49889617799752983 ) ) ;
#4136 = AXIS2_PLACEMENT_3D ( 'NONE', #1466, #2547, #40 ) ;
#4137 = CARTESIAN_POINT ( 'NONE',  ( 7.620005009003977037, 6.397500832047211539, 18.40096039353565160 ) ) ;
#4138 = VECTOR ( 'NONE', #1390, 1000.000000000000000 ) ;
#4139 = AXIS2_PLACEMENT_3D ( 'NONE', #2996, #4086, #1996 ) ;
#4140 = VERTEX_POINT ( 'NONE', #745 ) ;
#4141 = AXIS2_PLACEMENT_3D ( 'NONE', #4441, #4158, #1252 ) ;
#4142 = CARTESIAN_POINT ( 'NONE',  ( -3.573742765438046476, 0.004097986548672528061, 17.15262445358908039 ) ) ;
#4143 = AXIS2_PLACEMENT_3D ( 'NONE', #423, #2586, #4024 ) ;
#4144 = CIRCLE ( 'NONE', #2480, 0.7499999999999997780 ) ;
#4145 = DIRECTION ( 'NONE',  ( 0.000000000000000000, -1.000000000000000000, 0.000000000000000000 ) ) ;
#4146 = ORIENTED_EDGE ( 'NONE', *, *, #1174, .T. ) ;
#4147 = ORIENTED_EDGE ( 'NONE', *, *, #1247, .T. ) ;
#4148 = CARTESIAN_POINT ( 'NONE',  ( -13.93189556199112644, 3.198158771919405563, 38.77513429737268780 ) ) ;
#4149 = ADVANCED_FACE ( 'NONE', ( #1606 ), #1210, .F. ) ;
#4150 = DIRECTION ( 'NONE',  ( 1.000000000000000000, -1.076498916035107621E-16, -0.000000000000000000 ) ) ;
#4151 = UNCERTAINTY_MEASURE_WITH_UNIT (LENGTH_MEASURE( 1.000000000000000082E-05 ), #3277, 'distance_accuracy_value', 'NONE');
#4152 = ADVANCED_FACE ( 'NONE', ( #1631 ), #917, .F. ) ;
#4153 = ORIENTED_EDGE ( 'NONE', *, *, #2954, .T. ) ;
#4154 = DIRECTION ( 'NONE',  ( 1.000000000000000000, 0.000000000000000000, 0.000000000000000000 ) ) ;
#4155 = SHAPE_REPRESENTATION_RELATIONSHIP ( 'NONE' , 'NONE' ,  #1824, #323 ) ;
#4156 = DIRECTION ( 'NONE',  ( 0.000000000000000000, -1.000000000000000000, 0.000000000000000000 ) ) ;
#4157 = CARTESIAN_POINT ( 'NONE',  ( 14.16479065912717772, 1.882519613464290087, 39.26516300994396147 ) ) ;
#4158 = DIRECTION ( 'NONE',  ( 0.000000000000000000, -1.000000000000000000, 0.000000000000000000 ) ) ;
#4159 = DIRECTION ( 'NONE',  ( -1.355782318074878530E-16, -1.000000000000000000, 0.000000000000000000 ) ) ;
#4160 = CARTESIAN_POINT ( 'NONE',  ( -13.86261300049099709, -3.454607104308479393, 30.93839646180238745 ) ) ;
#4161 = ORIENTED_EDGE ( 'NONE', *, *, #2186, .F. ) ;
#4162 = CARTESIAN_POINT ( 'NONE',  ( -11.90638613189174144, -7.897499167952782173, 17.65096039353565160 ) ) ;
#4163 = ORIENTED_EDGE ( 'NONE', *, *, #3402, .F. ) ;
#4164 = CYLINDRICAL_SURFACE ( 'NONE', #4528, 0.5000000000000000000 ) ;
#4165 = EDGE_LOOP ( 'NONE', ( #1520, #3258, #3086, #2963 ) ) ;
#4166 = LINE ( 'NONE', #4210, #2523 ) ;
#4167 = EDGE_LOOP ( 'NONE', ( #3450, #1403, #3803, #529 ) ) ;
#4168 = EDGE_CURVE ( 'NONE', #1649, #2747, #2757, .T. ) ;
#4169 = ORIENTED_EDGE ( 'NONE', *, *, #251, .F. ) ;
#4170 = CARTESIAN_POINT ( 'NONE',  ( 7.234561953626996335E-06, 0.004097986548672528061, 3.292624453589077405 ) ) ;
#4171 = ORIENTED_EDGE ( 'NONE', *, *, #3501, .F. ) ;
#4172 = CARTESIAN_POINT ( 'NONE',  ( 18.74250723456195189, -3.569652013451328987, 31.86762445358909446 ) ) ;
#4173 = AXIS2_PLACEMENT_3D ( 'NONE', #3631, #1479, #1125 ) ;
#4174 = DIRECTION ( 'NONE',  ( -0.5448695207807678909, -2.428612866367529932E-17, 0.8385208437028482953 ) ) ;
#4175 = CARTESIAN_POINT ( 'NONE',  ( -12.87895030840308230, -6.192406806261855579, 35.96538579746959385 ) ) ;
#4176 = CARTESIAN_POINT ( 'NONE',  ( 13.23919053713719407, -5.374173505363492254, 37.08379739163954980 ) ) ;
#4177 = CARTESIAN_POINT ( 'NONE',  ( -14.28750000000000142, -3.249382362871961689E-18, 131.2499999999999716 ) ) ;
#4178 = AXIS2_PLACEMENT_3D ( 'NONE', #2202, #1857, #2176 ) ;
#4179 = CARTESIAN_POINT ( 'NONE',  ( 14.28168039487356289, -0.4681722336210599189, 35.91662862617997121 ) ) ;
#4180 = CARTESIAN_POINT ( 'NONE',  ( 2.316727177394500794E-17, 0.000000000000000000, 11.11249999999999893 ) ) ;
#4181 = ORIENTED_EDGE ( 'NONE', *, *, #1834, .T. ) ;
#4182 = CARTESIAN_POINT ( 'NONE',  ( 6.586250505521797471, -12.25345428146915161, 13.73375050552179566 ) ) ;
#4183 = AXIS2_PLACEMENT_3D ( 'NONE', #1585, #168, #2630 ) ;
#4184 = ADVANCED_FACE ( 'NONE', ( #1955 ), #2292, .F. ) ;
#4185 = ORIENTED_EDGE ( 'NONE', *, *, #404, .T. ) ;
#4186 = AXIS2_PLACEMENT_3D ( 'NONE', #4492, #4418, #1206 ) ;
#4187 = CARTESIAN_POINT ( 'NONE',  ( 12.87888252809135459, -6.188448225968623539, 35.46669787887593372 ) ) ;
#4188 = EDGE_CURVE ( 'NONE', #2437, #2372, #3758, .T. ) ;
#4189 = DIRECTION ( 'NONE',  ( -1.076498916035107621E-16, 1.000000000000000000, 0.000000000000000000 ) ) ;
#4190 = ORIENTED_EDGE ( 'NONE', *, *, #3169, .T. ) ;
#4191 = ORIENTED_EDGE ( 'NONE', *, *, #456, .F. ) ;
#4192 = AXIS2_PLACEMENT_3D ( 'NONE', #3664, #439, #4304 ) ;
#4193 = CARTESIAN_POINT ( 'NONE',  ( 17.28000050552179800, -17.78000000000000114, 17.78000050552179445 ) ) ;
#4194 = ORIENTED_EDGE ( 'NONE', *, *, #2821, .F. ) ;
#4195 = CARTESIAN_POINT ( 'NONE',  ( 2.316727177394500794E-17, 0.000000000000000000, 11.11249999999999893 ) ) ;
#4196 = EDGE_CURVE ( 'NONE', #1630, #254, #559, .T. ) ;
#4197 = CARTESIAN_POINT ( 'NONE',  ( -13.83081082357190361, -3.605823043002055694, 38.55467339862568110 ) ) ;
#4198 = FACE_OUTER_BOUND ( 'NONE', #4504, .T. ) ;
#4199 = CARTESIAN_POINT ( 'NONE',  ( -14.28749276543804925, 0.004097986548672528061, 39.01512445358908820 ) ) ;
#4200 = CIRCLE ( 'NONE', #2917, 0.5000000000000000000 ) ;
#4201 = DIRECTION ( 'NONE',  ( -1.000000000000000000, 0.000000000000000000, -0.000000000000000000 ) ) ;
#4202 = CARTESIAN_POINT ( 'NONE',  ( 10.16000050552179701, -10.16000000000000014, 17.78000050552179445 ) ) ;
#4203 = VERTEX_POINT ( 'NONE', #2720 ) ;
#4204 = LINE ( 'NONE', #2454, #3159 ) ;
#4205 = CARTESIAN_POINT ( 'NONE',  ( 7.234561953626996335E-06, 0.004097986548672528061, 17.16762445358907385 ) ) ;
#4206 = ADVANCED_FACE ( 'NONE', ( #4063 ), #4445, .T. ) ;
#4207 = VECTOR ( 'NONE', #716, 1000.000000000000000 ) ;
#4208 = VERTEX_POINT ( 'NONE', #1558 ) ;
#4209 = CARTESIAN_POINT ( 'NONE',  ( 13.48425643984108468, -4.722725237461219194, 37.23391125615015795 ) ) ;
#4210 = CARTESIAN_POINT ( 'NONE',  ( 3.749999999999999556, 3.750000000000000000, 3.749999999999995559 ) ) ;
#4211 = ORIENTED_EDGE ( 'NONE', *, *, #105, .T. ) ;
#4212 = ORIENTED_EDGE ( 'NONE', *, *, #3999, .T. ) ;
#4213 = TOROIDAL_SURFACE ( 'NONE', #4595, 1.500000000000000000, 0.7500000000000000000 ) ;
#4214 = SURFACE_SIDE_STYLE ('',( #3858 ) ) ;
#4215 = COLOUR_RGB ( '', 0.08235294, 0.09019608, 0.10196078) ;
#4216 = EDGE_CURVE ( 'NONE', #1569, #4, #3436, .T. ) ;
#4217 = ORIENTED_EDGE ( 'NONE', *, *, #4225, .T. ) ;
#4218 = CARTESIAN_POINT ( 'NONE',  ( 7.234561953626996335E-06, 0.004097986548672528061, -10.04237554641092345 ) ) ;
#4219 = FACE_OUTER_BOUND ( 'NONE', #1315, .T. ) ;
#4220 = FACE_OUTER_BOUND ( 'NONE', #4641, .T. ) ;
#4221 = DIRECTION ( 'NONE',  ( -0.000000000000000000, -0.000000000000000000, 1.000000000000000000 ) ) ;
#4222 = DIRECTION ( 'NONE',  ( -1.000000000000000000, -0.000000000000000000, -0.000000000000000000 ) ) ;
#4223 = ADVANCED_FACE ( 'NONE', ( #3383 ), #2627, .T. ) ;
#4224 = CARTESIAN_POINT ( 'NONE',  ( -14.20090685550316323, -1.581291399450686752, 28.65630886300585800 ) ) ;
#4225 = EDGE_CURVE ( 'NONE', #3620, #2014, #4112, .T. ) ;
#4226 = DIRECTION ( 'NONE',  ( 9.517981353260378315E-33, -8.841607930564763213E-17, 1.000000000000000000 ) ) ;
#4227 = DIRECTION ( 'NONE',  ( -1.000000000000000000, -0.000000000000000000, -0.000000000000000000 ) ) ;
#4228 = DIRECTION ( 'NONE',  ( 0.000000000000000000, 0.000000000000000000, -1.000000000000000000 ) ) ;
#4229 = PRESENTATION_LAYER_ASSIGNMENT (  '', '', ( #1237 ) ) ;
#4230 = EDGE_CURVE ( 'NONE', #2126, #3252, #1579, .T. ) ;
#4231 = ORIENTED_EDGE ( 'NONE', *, *, #2855, .T. ) ;
#4232 = FACE_OUTER_BOUND ( 'NONE', #103, .T. ) ;
#4233 = TOROIDAL_SURFACE ( 'NONE', #4311, 1.500000000000000000, 0.7500000000000000000 ) ;
#4234 = DIRECTION ( 'NONE',  ( -0.000000000000000000, -0.000000000000000000, -1.000000000000000000 ) ) ;
#4235 = CYLINDRICAL_SURFACE ( 'NONE', #101, 0.7499999999999997780 ) ;
#4236 = ORIENTED_EDGE ( 'NONE', *, *, #265, .F. ) ;
#4237 = ORIENTED_EDGE ( 'NONE', *, *, #2346, .F. ) ;
#4238 = LINE ( 'NONE', #1359, #2649 ) ;
#4239 = ORIENTED_EDGE ( 'NONE', *, *, #3402, .T. ) ;
#4240 = DIRECTION ( 'NONE',  ( 1.000000000000000000, 0.000000000000000000, 0.000000000000000000 ) ) ;
#4241 = ORIENTED_EDGE ( 'NONE', *, *, #1582, .F. ) ;
#4242 = CARTESIAN_POINT ( 'NONE',  ( -7.619992765438044380, 12.08996809382683857, 17.90262445358908039 ) ) ;
#4243 =( NAMED_UNIT ( * ) SI_UNIT ( $, .STERADIAN. ) SOLID_ANGLE_UNIT ( ) );
#4244 = CARTESIAN_POINT ( 'NONE',  ( -11.90638390633376531, 7.901597986548672736, 17.15262445358908039 ) ) ;
#4245 = CARTESIAN_POINT ( 'NONE',  ( -9.549434556529077899E-17, -3.249382362871961689E-18, 131.2499999999999716 ) ) ;
#4246 = LINE ( 'NONE', #1677, #2912 ) ;
#4247 = B_SPLINE_CURVE_WITH_KNOTS ( 'NONE', 3,
 ( #625, #4609, #4179, #3123, #980, #1656, #2424, #962, #2379, #2067, #3502, #2356, #1394, #2402, #1999, #3802, #3845, #2809 ),
 .UNSPECIFIED., .F., .F.,
 ( 4, 2, 2, 2, 2, 2, 2, 2, 4 ),
 ( 0.01682620116816211167, 0.01752698813223788760, 0.01822777509631366005, 0.01892856206038943598, 0.01962934902446520843, 0.02033013598854098436, 0.02103092295261676029, 0.02173170991669253621, 0.02243249688076830867 ),
 .UNSPECIFIED. ) ;
#4248 = AXIS2_PLACEMENT_3D ( 'NONE', #1459, #730, #317 ) ;
#4249 = DIRECTION ( 'NONE',  ( -1.000000000000000000, -0.000000000000000000, -0.000000000000000000 ) ) ;
#4250 = CARTESIAN_POINT ( 'NONE',  ( -3.750000000000000888, -3.750000000000000000, 3.749999999999995559 ) ) ;
#4251 = CARTESIAN_POINT ( 'NONE',  ( -12.02319158376690567, -7.719183544751668791, 17.66665972527254880 ) ) ;
#4252 = CARTESIAN_POINT ( 'NONE',  ( 10.16000050552179701, -13.73374999999999879, 10.16000050552179701 ) ) ;
#4253 = CARTESIAN_POINT ( 'NONE',  ( -7.619992765438044380, 6.401597986548673624, 31.86762445358908735 ) ) ;
#4254 = ADVANCED_FACE ( 'NONE', ( #4468 ), #134, .F. ) ;
#4255 = VERTEX_POINT ( 'NONE', #1256 ) ;
#4256 = CARTESIAN_POINT ( 'NONE',  ( 12.47855123652872322, -6.954457826542711274, 33.51726641232498594 ) ) ;
#4257 = CIRCLE ( 'NONE', #1414, 1.499999999999999556 ) ;
#4258 = ADVANCED_FACE ( 'NONE', ( #3050 ), #160, .F. ) ;
#4259 = CARTESIAN_POINT ( 'NONE',  ( 2.540000505521796015, -17.28000000000000114, 17.78000050552179445 ) ) ;
#4260 = VECTOR ( 'NONE', #3696, 1000.000000000000000 ) ;
#4261 = ORIENTED_EDGE ( 'NONE', *, *, #900, .T. ) ;
#4262 = VERTEX_POINT ( 'NONE', #890 ) ;
#4263 = VECTOR ( 'NONE', #988, 1000.000000000000000 ) ;
#4264 = ORIENTED_EDGE ( 'NONE', *, *, #303, .T. ) ;
#4265 = DIRECTION ( 'NONE',  ( -1.000000000000000000, 0.000000000000000000, 0.000000000000000000 ) ) ;
#4266 = ORIENTED_EDGE ( 'NONE', *, *, #1375, .T. ) ;
#4267 = DIRECTION ( 'NONE',  ( -1.000000000000000000, 0.000000000000000000, 0.000000000000000000 ) ) ;
#4268 = CARTESIAN_POINT ( 'NONE',  ( -14.24206966858596068, -1.158719165697675635, 35.75466352049880214 ) ) ;
#4269 = CARTESIAN_POINT ( 'NONE',  ( 12.37117714425454551, -7.147499167952787502, 32.84705871297352076 ) ) ;
#4270 = CARTESIAN_POINT ( 'NONE',  ( 8.370007234561949616, 6.401597986548672736, 17.90262445358908039 ) ) ;
#4271 = AXIS2_PLACEMENT_3D ( 'NONE', #1984, #1871, #3763 ) ;
#4272 = FACE_OUTER_BOUND ( 'NONE', #4471, .T. ) ;
#4273 = CARTESIAN_POINT ( 'NONE',  ( 7.234561953626996335E-06, 0.004097986548672528061, -1.469875546410923661 ) ) ;
#4274 = CARTESIAN_POINT ( 'NONE',  ( -3.262492765438076869, 0.004097986548673020722, -10.04237554641092345 ) ) ;
#4275 = DIRECTION ( 'NONE',  ( 1.000000000000000000, 0.000000000000000000, -0.000000000000000000 ) ) ;
#4276 = EDGE_CURVE ( 'NONE', #2052, #696, #4306, .T. ) ;
#4277 = CIRCLE ( 'NONE', #2463, 0.7500000000000006661 ) ;
#4278 = ORIENTED_EDGE ( 'NONE', *, *, #4608, .T. ) ;
#4279 = CARTESIAN_POINT ( 'NONE',  ( 12.51138117596144994, -6.895500623138680396, 33.74860486214564048 ) ) ;
#4280 = CARTESIAN_POINT ( 'NONE',  ( 17.78000050552179445, -2.539999999999999591, 3.040000505521795571 ) ) ;
#4281 = EDGE_CURVE ( 'NONE', #2642, #359, #2109, .T. ) ;
#4282 = ORIENTED_EDGE ( 'NONE', *, *, #2893, .T. ) ;
#4283 = ORIENTED_EDGE ( 'NONE', *, *, #4345, .F. ) ;
#4284 = LINE ( 'NONE', #704, #1360 ) ;
#4285 = AXIS2_PLACEMENT_3D ( 'NONE', #3167, #4605, #2085 ) ;
#4286 = EDGE_LOOP ( 'NONE', ( #549, #3003 ) ) ;
#4287 = DIRECTION ( 'NONE',  ( 1.000000000000000000, 0.000000000000000000, 0.000000000000000000 ) ) ;
#4288 = ORIENTED_EDGE ( 'NONE', *, *, #4091, .T. ) ;
#4289 = DIRECTION ( 'NONE',  ( 8.673617379884027583E-16, 0.000000000000000000, 1.000000000000000000 ) ) ;
#4290 = EDGE_CURVE ( 'NONE', #971, #4494, #2787, .T. ) ;
#4291 = DIRECTION ( 'NONE',  ( 0.9751221211376644993, -1.734723475976807094E-18, -0.2216683307736626585 ) ) ;
#4292 = STYLED_ITEM ( 'NONE', ( #226 ), #1876 ) ;
#4293 = CARTESIAN_POINT ( 'NONE',  ( -11.90638613189173789, 7.897500832047212427, 17.65096039353565160 ) ) ;
#4294 = CARTESIAN_POINT ( 'NONE',  ( 14.19373809557357191, 1.654917666244543284, 38.82591248395576855 ) ) ;
#4295 = EDGE_CURVE ( 'NONE', #3952, #2867, #964, .T. ) ;
#4296 = AXIS2_PLACEMENT_3D ( 'NONE', #409, #3913, #2872 ) ;
#4297 = LINE ( 'NONE', #2473, #3414 ) ;
#4298 = CARTESIAN_POINT ( 'NONE',  ( 8.370005009003978813, 7.147500832047211539, 18.40096039353565160 ) ) ;
#4299 = CARTESIAN_POINT ( 'NONE',  ( 2.540000505521796015, -10.16000000000000014, 10.16000050552179701 ) ) ;
#4300 = CARTESIAN_POINT ( 'NONE',  ( 17.78000050552179445, -10.16000000000000014, 10.16000050552179701 ) ) ;
#4301 = DIRECTION ( 'NONE',  ( 1.000000000000000000, -1.076498916035107744E-16, -0.000000000000000000 ) ) ;
#4302 = AXIS2_PLACEMENT_3D ( 'NONE', #3052, #1279, #2700 ) ;
#4303 = EDGE_LOOP ( 'NONE', ( #2929, #3922, #1823, #2237 ) ) ;
#4304 = DIRECTION ( 'NONE',  ( 1.000000000000000000, 0.000000000000000000, -0.000000000000000000 ) ) ;
#4305 = CARTESIAN_POINT ( 'NONE',  ( -12.37116490068861374, -7.143402013451327193, 32.34863974131315700 ) ) ;
#4306 = B_SPLINE_CURVE_WITH_KNOTS ( 'NONE', 3,
 ( #864, #539, #1979, #4135, #4495, #2002, #1278, #1746, #3503, #3805 ),
 .UNSPECIFIED., .F., .F.,
 ( 4, 2, 2, 2, 4 ),
 ( 0.000000000000000000, 0.0003199342119934982936, 0.0006398684239869965873, 0.0009598026359804948809, 0.001279736847973993175 ),
 .UNSPECIFIED. ) ;
#4307 = DIRECTION ( 'NONE',  ( 0.000000000000000000, -1.000000000000000000, 0.000000000000000000 ) ) ;
#4308 = EDGE_LOOP ( 'NONE', ( #2405, #3971, #1334, #2990 ) ) ;
#4309 = ORIENTED_EDGE ( 'NONE', *, *, #1699, .T. ) ;
#4310 = CARTESIAN_POINT ( 'NONE',  ( -13.30083662496763530, 5.224265971132247444, 36.75526953962744869 ) ) ;
#4311 = AXIS2_PLACEMENT_3D ( 'NONE', #841, #867, #2277 ) ;
#4312 = EDGE_CURVE ( 'NONE', #421, #1822, #510, .T. ) ;
#4313 = EDGE_LOOP ( 'NONE', ( #904, #2961 ) ) ;
#4314 = ORIENTED_EDGE ( 'NONE', *, *, #2041, .T. ) ;
#4315 = CARTESIAN_POINT ( 'NONE',  ( -14.00292651309607095, 2.844510957948676033, 29.68641762507535020 ) ) ;
#4316 = SHAPE_DEFINITION_REPRESENTATION ( #3508, #2796 ) ;
#4317 = CARTESIAN_POINT ( 'NONE',  ( -3.749994990996019517, 3.750000832047212906, 18.79096039353565217 ) ) ;
#4318 = DIRECTION ( 'NONE',  ( 0.000000000000000000, -0.000000000000000000, -1.000000000000000000 ) ) ;
#4319 = DIRECTION ( 'NONE',  ( 0.000000000000000000, 0.000000000000000000, 1.000000000000000000 ) ) ;
#4320 = APPLICATION_CONTEXT ( 'automotive_design' ) ;
#4321 = CARTESIAN_POINT ( 'NONE',  ( -14.28749276543804925, 0.004097986548672528061, 3.292624453589077405 ) ) ;
#4322 = DIRECTION ( 'NONE',  ( 1.000000000000000000, 0.000000000000000000, -0.000000000000000000 ) ) ;
#4323 = CARTESIAN_POINT ( 'NONE',  ( 13.92261338244811952, -3.205599502867460870, 33.45626019218369862 ) ) ;
#4324 = SURFACE_STYLE_USAGE ( .BOTH. , #1882 ) ;
#4325 = DIRECTION ( 'NONE',  ( 0.000000000000000000, -1.000000000000000000, -0.000000000000000000 ) ) ;
#4326 = ORIENTED_EDGE ( 'NONE', *, *, #1276, .T. ) ;
#4327 = CARTESIAN_POINT ( 'NONE',  ( 14.17575158735941088, 1.794122187399060930, 35.46543942424121809 ) ) ;
#4328 = PRODUCT_DEFINITION_FORMATION_WITH_SPECIFIED_SOURCE ( 'ANY', '', #3876, .NOT_KNOWN. ) ;
#4329 = DIRECTION ( 'NONE',  ( -2.312964634635740689E-15, 0.000000000000000000, -1.000000000000000000 ) ) ;
#4330 = EDGE_CURVE ( 'NONE', #2464, #209, #3462, .T. ) ;
#4331 = DIRECTION ( 'NONE',  ( -1.000000000000000000, -8.673617379884035472E-17, 0.000000000000000000 ) ) ;
#4332 = VERTEX_POINT ( 'NONE', #1004 ) ;
#4333 = AXIS2_PLACEMENT_3D ( 'NONE', #1610, #2280, #4068 ) ;
#4334 = ORIENTED_EDGE ( 'NONE', *, *, #361, .F. ) ;
#4335 = EDGE_CURVE ( 'NONE', #245, #2747, #1637, .T. ) ;
#4336 = ORIENTED_EDGE ( 'NONE', *, *, #1303, .T. ) ;
#4337 = ORIENTED_EDGE ( 'NONE', *, *, #4330, .F. ) ;
#4338 = CARTESIAN_POINT ( 'NONE',  ( -14.24246428466184078, 1.158051217861460591, 28.47725504917529804 ) ) ;
#4339 = APPLICATION_PROTOCOL_DEFINITION ( 'draft international standard', 'automotive_design', 1998, #1297 ) ;
#4340 = CARTESIAN_POINT ( 'NONE',  ( 1.130815084004146875, -3.565902013451327068, -9.569796636679910762 ) ) ;
#4341 = CARTESIAN_POINT ( 'NONE',  ( -13.83947321077509329, 3.550175980372930251, 31.89403414396633352 ) ) ;
#4342 = DIRECTION ( 'NONE',  ( -0.000000000000000000, -0.000000000000000000, -1.000000000000000000 ) ) ;
#4343 = AXIS2_PLACEMENT_3D ( 'NONE', #3923, #2117, #331 ) ;
#4344 = LINE ( 'NONE', #1880, #4207 ) ;
#4345 = EDGE_CURVE ( 'NONE', #2227, #2910, #2220, .T. ) ;
#4346 = CARTESIAN_POINT ( 'NONE',  ( -6.869994990996018736, 12.08587093932537826, 18.40096039353565160 ) ) ;
#4347 = CIRCLE ( 'NONE', #2533, 0.5000000000000004441 ) ;
#4348 = CYLINDRICAL_SURFACE ( 'NONE', #2155, 0.5000000000000000000 ) ;
#4349 = ORIENTED_EDGE ( 'NONE', *, *, #870, .F. ) ;
#4350 = PLANE ( 'NONE',  #4192 ) ;
#4351 = CARTESIAN_POINT ( 'NONE',  ( 3.040000505521796015, -17.28000000000000114, 3.040000505521796015 ) ) ;
#4352 = EDGE_CURVE ( 'NONE', #3350, #3489, #2818, .T. ) ;
#4353 = VECTOR ( 'NONE', #2759, 1000.000000000000000 ) ;
#4354 = EDGE_CURVE ( 'NONE', #4255, #1351, #229, .T. ) ;
#4355 = CARTESIAN_POINT ( 'NONE',  ( 17.28000050552179445, -3.039999999999999591, 3.040000505521796015 ) ) ;
#4356 = EDGE_LOOP ( 'NONE', ( #242, #876, #4601, #480 ) ) ;
#4357 = AXIS2_PLACEMENT_3D ( 'NONE', #1939, #118, #845 ) ;
#4358 = ORIENTED_EDGE ( 'NONE', *, *, #2450, .T. ) ;
#4359 = CARTESIAN_POINT ( 'NONE',  ( -13.93189333643315564, 3.202255926420866761, 38.27679835742612369 ) ) ;
#4360 = ORIENTED_EDGE ( 'NONE', *, *, #2959, .F. ) ;
#4361 = VERTEX_POINT ( 'NONE', #4560 ) ;
#4362 = AXIS2_PLACEMENT_3D ( 'NONE', #1772, #2133, #3196 ) ;
#4363 = CARTESIAN_POINT ( 'NONE',  ( -14.28749499099602005, 8.320472128100606877E-07, 39.51346039353565942 ) ) ;
#4364 = SHAPE_DEFINITION_REPRESENTATION ( #989, #4401 ) ;
#4365 = CARTESIAN_POINT ( 'NONE',  ( -2.677025490679457498, -3.565902013451327068, -8.856895997200147974 ) ) ;
#4366 = VECTOR ( 'NONE', #1791, 1000.000000000000000 ) ;
#4367 = VECTOR ( 'NONE', #2717, 1000.000000000000000 ) ;
#4368 = CARTESIAN_POINT ( 'NONE',  ( -13.86261522604896257, -3.458704258809938370, 31.43673240174894801 ) ) ;
#4369 = AXIS2_PLACEMENT_3D ( 'NONE', #652, #1722, #3506 ) ;
#4370 = FACE_OUTER_BOUND ( 'NONE', #1427, .T. ) ;
#4371 = PLANE ( 'NONE',  #1583 ) ;
#4372 = VECTOR ( 'NONE', #2496, 1000.000000000000000 ) ;
#4373 = DIRECTION ( 'NONE',  ( -0.000000000000000000, -0.000000000000000000, -1.000000000000000000 ) ) ;
#4374 = LINE ( 'NONE', #1161, #164 ) ;
#4375 = EDGE_CURVE ( 'NONE', #356, #992, #2069, .T. ) ;
#4376 = CARTESIAN_POINT ( 'NONE',  ( 14.28750723456195715, -0.2301263156859972014, 28.29387445358909758 ) ) ;
#4377 = ORIENTED_EDGE ( 'NONE', *, *, #1508, .T. ) ;
#4378 = DIRECTION ( 'NONE',  ( -1.000000000000000000, -1.707404996040164265E-16, 0.000000000000000000 ) ) ;
#4379 = CARTESIAN_POINT ( 'NONE',  ( -12.58213841360289820, -6.768164877760692200, 34.20015322194398522 ) ) ;
#4380 = CARTESIAN_POINT ( 'NONE',  ( 2.316727177394501718E-17, 0.000000000000000000, 33.33750000000000568 ) ) ;
#4381 = EDGE_LOOP ( 'NONE', ( #1404, #1046, #627, #3117 ) ) ;
#4382 = DIRECTION ( 'NONE',  ( -0.000000000000000000, -0.000000000000000000, -1.000000000000000000 ) ) ;
#4383 = DIRECTION ( 'NONE',  ( 1.000000000000000000, -1.076498916035107621E-16, -0.000000000000000000 ) ) ;
#4384 = DIRECTION ( 'NONE',  ( 1.000000000000000000, -1.076498916035107744E-16, 0.000000000000000000 ) ) ;
#4385 = VERTEX_POINT ( 'NONE', #3526 ) ;
#4386 = ORIENTED_EDGE ( 'NONE', *, *, #3658, .T. ) ;
#4387 = CARTESIAN_POINT ( 'NONE',  ( -14.20057228749327827, 1.588540649541856808, 35.57580161124558060 ) ) ;
#4388 = CONTEXT_DEPENDENT_SHAPE_REPRESENTATION ( #2475, #238 ) ;
#4389 = CIRCLE ( 'NONE', #3491, 4.762499999999999289 ) ;
#4390 = LINE ( 'NONE', #4410, #4069 ) ;
#4391 = ORIENTED_EDGE ( 'NONE', *, *, #4188, .T. ) ;
#4392 = CARTESIAN_POINT ( 'NONE',  ( -12.37116712624657033, 7.147500832047212427, 32.36596039353565857 ) ) ;
#4393 = CARTESIAN_POINT ( 'NONE',  ( -13.83332089671217169, -3.569652013451326322, 31.86762445358909446 ) ) ;
#4394 = LINE ( 'NONE', #1181, #4431 ) ;
#4395 = CARTESIAN_POINT ( 'NONE',  ( -14.25898534185092004, -0.9269869019229697304, 35.32593247230593647 ) ) ;
#4396 = CARTESIAN_POINT ( 'NONE',  ( 12.02324309811277203, -7.719128299133020121, 17.66658805193229753 ) ) ;
#4397 = VERTEX_POINT ( 'NONE', #649 ) ;
#4398 = CARTESIAN_POINT ( 'NONE',  ( 13.85858657070305711, 3.479382377821004013, 33.30553846872138024 ) ) ;
#4399 = CARTESIAN_POINT ( 'NONE',  ( -14.28749276543804037, -0.4768660484013518830, 39.01512445358906689 ) ) ;
#4400 = CYLINDRICAL_SURFACE ( 'NONE', #3109, 7.147499999999999076 ) ;
#4401 = SHAPE_REPRESENTATION ( 'MAS-681', ( #3127, #3041, #2361, #1556, #2591, #1851, #491, #342, #4248, #4173, #946, #1331, #1258, #2431 ), #2509 ) ;
#4402 = VERTEX_POINT ( 'NONE', #3846 ) ;
#4403 = CARTESIAN_POINT ( 'NONE',  ( 13.73375050552179744, -10.16000000000000014, 13.73375050552179744 ) ) ;
#4404 = EDGE_CURVE ( 'NONE', #3559, #21, #790, .T. ) ;
#4405 = LINE ( 'NONE', #872, #915 ) ;
#4406 = CARTESIAN_POINT ( 'NONE',  ( 17.78000050552179445, -10.16000000000000014, 13.73375050552179744 ) ) ;
#4407 = ORIENTED_EDGE ( 'NONE', *, *, #871, .T. ) ;
#4408 = CARTESIAN_POINT ( 'NONE',  ( -7.619994990996017847, 6.397500832047212427, 32.36596039353565857 ) ) ;
#4409 = AXIS2_PLACEMENT_3D ( 'NONE', #1937, #95, #1542 ) ;
#4410 = CARTESIAN_POINT ( 'NONE',  ( 8.370007234561949616, -7.893402013451324528, 17.15262445358908039 ) ) ;
#4411 = ORIENTED_EDGE ( 'NONE', *, *, #3386, .F. ) ;
#4412 = AXIS2_PLACEMENT_3D ( 'NONE', #509, #2973, #1953 ) ;
#4413 = DIRECTION ( 'NONE',  ( 0.000000000000000000, -1.000000000000000000, 0.000000000000000000 ) ) ;
#4414 = AXIS2_PLACEMENT_3D ( 'NONE', #4102, #3701, #3348 ) ;
#4415 = CYLINDRICAL_SURFACE ( 'NONE', #3825, 3.573749999999999538 ) ;
#4416 = CARTESIAN_POINT ( 'NONE',  ( -13.87980694821278149, -3.385868028865885115, 33.02271771428084435 ) ) ;
#4417 = CARTESIAN_POINT ( 'NONE',  ( -12.35745565209315444, 7.171352271666981970, 18.18649461234914710 ) ) ;
#4418 = DIRECTION ( 'NONE',  ( -0.000000000000000000, -0.000000000000000000, -1.000000000000000000 ) ) ;
#4419 = AXIS2_PLACEMENT_3D ( 'NONE', #2699, #2275, #2338 ) ;
#4420 = ORIENTED_EDGE ( 'NONE', *, *, #13, .F. ) ;
#4421 = DIRECTION ( 'NONE',  ( 1.000000000000000000, 0.000000000000000000, 0.000000000000000000 ) ) ;
#4422 = DIRECTION ( 'NONE',  ( 1.000000000000000000, -1.076498916035107621E-16, 0.000000000000000000 ) ) ;
#4423 = ADVANCED_FACE ( 'NONE', ( #2404 ), #253, .F. ) ;
#4424 = ORIENTED_EDGE ( 'NONE', *, *, #105, .F. ) ;
#4425 = CARTESIAN_POINT ( 'NONE',  ( 14.00292109500077231, -2.836439352166247208, 29.68646118753943952 ) ) ;
#4426 = CARTESIAN_POINT ( 'NONE',  ( 10.16000050552179701, -10.16000000000000014, 17.78000050552179445 ) ) ;
#4427 = DIRECTION ( 'NONE',  ( -1.000000000000000000, 8.673617379884035472E-17, 0.000000000000000000 ) ) ;
#4428 = EDGE_CURVE ( 'NONE', #1513, #1644, #2810, .T. ) ;
#4429 = EDGE_CURVE ( 'NONE', #44, #501, #4585, .T. ) ;
#4430 = ORIENTED_EDGE ( 'NONE', *, *, #1836, .F. ) ;
#4431 = VECTOR ( 'NONE', #4036, 1000.000000000000000 ) ;
#4432 = ORIENTED_EDGE ( 'NONE', *, *, #1103, .F. ) ;
#4433 = ITEM_DEFINED_TRANSFORMATION ( 'NONE', 'NONE', #1258,  #4483 ) ;
#4434 = LINE ( 'NONE', #525, #2371 ) ;
#4435 = ADVANCED_FACE ( 'NONE', ( #626 ), #2762, .F. ) ;
#4436 = ORIENTED_EDGE ( 'NONE', *, *, #2510, .F. ) ;
#4437 = DIRECTION ( 'NONE',  ( -1.000000000000000000, -1.076498916035107621E-16, 0.000000000000000000 ) ) ;
#4438 =( NAMED_UNIT ( * ) PLANE_ANGLE_UNIT ( ) SI_UNIT ( $, .RADIAN. ) );
#4439 = DIRECTION ( 'NONE',  ( 0.000000000000000000, -1.000000000000000000, 0.000000000000000000 ) ) ;
#4440 = PLANE ( 'NONE',  #305 ) ;
#4441 = CARTESIAN_POINT ( 'NONE',  ( 3.040000505521796015, -17.28000000000000114, 17.28000050552179445 ) ) ;
#4442 = DIRECTION ( 'NONE',  ( -1.000000000000000000, 1.076498916035107621E-16, 0.000000000000000000 ) ) ;
#4443 = B_SPLINE_CURVE_WITH_KNOTS ( 'NONE', 3,
 ( #3464, #3362, #1956, #1257, #3733, #4093, #3413, #3785, #840, #2672, #513, #165, #1607, #1211, #3079, #2276, #3025, #231 ),
 .UNSPECIFIED., .F., .F.,
 ( 4, 2, 2, 2, 2, 2, 2, 2, 4 ),
 ( 0.005610345619348811042, 0.006311274135232913807, 0.007012202651117017439, 0.007713131167001120204, 0.008414059682885222102, 0.009114988198769324867, 0.009815916714653427633, 0.01051684523053753040, 0.01121777374642162275 ),
 .UNSPECIFIED. ) ;
#4444 = EDGE_LOOP ( 'NONE', ( #1328, #3557, #287, #315 ) ) ;
#4445 = PLANE ( 'NONE',  #1199 ) ;
#4446 = VECTOR ( 'NONE', #4491, 1000.000000000000000 ) ;
#4447 = CARTESIAN_POINT ( 'NONE',  ( 18.74250723456195189, 0.004097986548670510577, 31.86762445358909446 ) ) ;
#4448 = ORIENTED_EDGE ( 'NONE', *, *, #1440, .F. ) ;
#4449 = DIRECTION ( 'NONE',  ( -1.000000000000000000, 0.000000000000000000, 0.000000000000000000 ) ) ;
#4450 = AXIS2_PLACEMENT_3D ( 'NONE', #1809, #4318, #1852 ) ;
#4451 = CYLINDRICAL_SURFACE ( 'NONE', #240, 3.573749999999999538 ) ;
#4452 = DIRECTION ( 'NONE',  ( 0.000000000000000000, 1.000000000000000000, 0.000000000000000000 ) ) ;
#4453 = CARTESIAN_POINT ( 'NONE',  ( 14.09171737252990653, 2.367226359320930396, 34.55865096437416639 ) ) ;
#4454 = VERTEX_POINT ( 'NONE', #981 ) ;
#4455 = ORIENTED_EDGE ( 'NONE', *, *, #3793, .T. ) ;
#4456 = CONTEXT_DEPENDENT_SHAPE_REPRESENTATION ( #3833, #2032 ) ;
#4457 = CARTESIAN_POINT ( 'NONE',  ( 13.87971526468629690, 3.390392411081628143, 31.21208060327063194 ) ) ;
#4458 = CARTESIAN_POINT ( 'NONE',  ( -7.619992765438045268, 0.004097986548673348585, 31.86762445358908735 ) ) ;
#4459 = COLOUR_RGB ( '', 0.31764706, 0.68627451, 0.89019608) ;
#4460 = ORIENTED_EDGE ( 'NONE', *, *, #2531, .F. ) ;
#4461 = CARTESIAN_POINT ( 'NONE',  ( 11.90639837545767321, 7.901597986548669184, 17.15262445358908039 ) ) ;
#4462 = DIRECTION ( 'NONE',  ( -1.000000000000000000, 0.000000000000000000, 0.000000000000000000 ) ) ;
#4463 = FACE_OUTER_BOUND ( 'NONE', #2729, .T. ) ;
#4464 = CARTESIAN_POINT ( 'NONE',  ( 12.76962709079479019, 6.411762314134477947, 35.55869424641613818 ) ) ;
#4465 = DIRECTION ( 'NONE',  ( -1.000000000000000000, 0.000000000000000000, 0.000000000000000000 ) ) ;
#4466 = FACE_OUTER_BOUND ( 'NONE', #1867, .T. ) ;
#4467 = ORIENTED_EDGE ( 'NONE', *, *, #2840, .F. ) ;
#4468 = FACE_OUTER_BOUND ( 'NONE', #815, .T. ) ;
#4469 = CARTESIAN_POINT ( 'NONE',  ( -12.37116490068861197, -7.143402013451321864, 17.90262445358908039 ) ) ;
#4470 = DIRECTION ( 'NONE',  ( -0.000000000000000000, -0.000000000000000000, 1.000000000000000000 ) ) ;
#4471 = EDGE_LOOP ( 'NONE', ( #2101, #908, #2004, #3702, #1432, #4570, #4194, #2383, #3302, #3975, #3781, #2748, #465, #350, #4076, #2339 ) ) ;
#4472 = CARTESIAN_POINT ( 'NONE',  ( 13.83943491502687628, -3.546271172620213186, 31.39737200185970067 ) ) ;
#4473 = CARTESIAN_POINT ( 'NONE',  ( -8.369994990996019624, -7.897499167952782173, 18.40096039353565160 ) ) ;
#4474 = PRODUCT_DEFINITION_CONTEXT ( 'detailed design', #3454, 'design' ) ;
#4475 = CARTESIAN_POINT ( 'NONE',  ( -7.619994990996017847, 6.397500832047212427, 32.36596039353565857 ) ) ;
#4476 = EDGE_CURVE ( 'NONE', #1212, #3252, #1847, .T. ) ;
#4477 = CARTESIAN_POINT ( 'NONE',  ( 6.586250505521797471, -8.066545718530848674, 13.73375050552179566 ) ) ;
#4478 = ORIENTED_EDGE ( 'NONE', *, *, #1763, .F. ) ;
#4479 = VERTEX_POINT ( 'NONE', #1104 ) ;
#4480 = ITEM_DEFINED_TRANSFORMATION ( 'NONE', 'NONE', #2431,  #4483 ) ;
#4481 = CARTESIAN_POINT ( 'NONE',  ( 13.83943987092327177, 3.550346313559760603, 31.89501272945897270 ) ) ;
#4482 = VECTOR ( 'NONE', #2585, 1000.000000000000000 ) ;
#4483 = AXIS2_PLACEMENT_3D ( 'NONE', #3752, #129, #3704 ) ;
#4484 = CARTESIAN_POINT ( 'NONE',  ( 3.573757234561953045, 0.004097986548672966078, 17.15262445358908039 ) ) ;
#4485 = UNCERTAINTY_MEASURE_WITH_UNIT (LENGTH_MEASURE( 1.000000000000000082E-05 ), #1364, 'distance_accuracy_value', 'NONE');
#4486 = ORIENTED_EDGE ( 'NONE', *, *, #4352, .F. ) ;
#4487 = CARTESIAN_POINT ( 'NONE',  ( 3.040000505521796015, -2.539999999999999591, 17.78000050552179445 ) ) ;
#4488 = AXIS2_PLACEMENT_3D ( 'NONE', #2846, #1045, #2100 ) ;
#4489 = CARTESIAN_POINT ( 'NONE',  ( -8.369994990996019624, -7.147499167952784838, 32.36596039353565857 ) ) ;
#4490 = PLANE ( 'NONE',  #2110 ) ;
#4491 = DIRECTION ( 'NONE',  ( 1.000000000000000000, -1.076498916035107744E-16, -0.000000000000000000 ) ) ;
#4492 = CARTESIAN_POINT ( 'NONE',  ( -8.369992765438043492, 6.401597986548673624, 17.90262445358908039 ) ) ;
#4493 = CIRCLE ( 'NONE', #2446, 3.573749999999998650 ) ;
#4494 = VERTEX_POINT ( 'NONE', #4012 ) ;
#4495 = CARTESIAN_POINT ( 'NONE',  ( 12.27095928922004653, -7.314612587678752220, 17.41568789468882983 ) ) ;
#4496 = ADVANCED_FACE ( 'NONE', ( #3941 ), #762, .T. ) ;
#4497 = VERTEX_POINT ( 'NONE', #2152 ) ;
#4498 = CYLINDRICAL_SURFACE ( 'NONE', #4072, 3.573749999999999538 ) ;
#4499 = VERTEX_POINT ( 'NONE', #2521 ) ;
#4500 = FACE_OUTER_BOUND ( 'NONE', #187, .T. ) ;
#4501 = EDGE_CURVE ( 'NONE', #2026, #1657, #1559, .T. ) ;
#4502 = VECTOR ( 'NONE', #2939, 1000.000000000000000 ) ;
#4503 = DIRECTION ( 'NONE',  ( -0.000000000000000000, -0.000000000000000000, -1.000000000000000000 ) ) ;
#4504 = EDGE_LOOP ( 'NONE', ( #2232, #774, #1235, #4161 ) ) ;
#4505 = VERTEX_POINT ( 'NONE', #4321 ) ;
#4506 = CARTESIAN_POINT ( 'NONE',  ( 14.20066698090924540, 1.587871178531814698, 29.15574023557984162 ) ) ;
#4507 = DIRECTION ( 'NONE',  ( 0.000000000000000000, -1.000000000000000000, 0.000000000000000000 ) ) ;
#4508 = VECTOR ( 'NONE', #4222, 1000.000000000000000 ) ;
#4509 = EDGE_LOOP ( 'NONE', ( #4358, #373, #4430, #3113 ) ) ;
#4510 = CARTESIAN_POINT ( 'NONE',  ( -7.619994990996019624, 3.573750832047213333, 32.36596039353566567 ) ) ;
#4511 = DIRECTION ( 'NONE',  ( 0.000000000000000000, 0.000000000000000000, 1.000000000000000000 ) ) ;
#4512 = DIRECTION ( 'NONE',  ( -1.000000000000000000, 8.673617379884035472E-17, 0.000000000000000000 ) ) ;
#4513 = CARTESIAN_POINT ( 'NONE',  ( 14.05881085617579629, 2.555481233519228734, 39.04506677964693750 ) ) ;
#4514 = CARTESIAN_POINT ( 'NONE',  ( -8.369994990996016071, 7.147500832047212427, 17.65096039353565160 ) ) ;
#4515 = CARTESIAN_POINT ( 'NONE',  ( -4.762492765438045339, 0.004097986548673111795, 3.292624453589077405 ) ) ;
#4516 = CARTESIAN_POINT ( 'NONE',  ( -13.94784670859836595, -3.095491346532870836, 30.07369728485308258 ) ) ;
#4517 = EDGE_LOOP ( 'NONE', ( #4122, #819, #2538, #2800 ) ) ;
#4518 = CARTESIAN_POINT ( 'NONE',  ( 3.573757234561953045, 0.004097986548672966078, 17.16762445358907385 ) ) ;
#4519 = DIRECTION ( 'NONE',  ( 0.000000000000000000, 0.000000000000000000, 1.000000000000000000 ) ) ;
#4520 = VERTEX_POINT ( 'NONE', #3634 ) ;
#4521 = PRESENTATION_LAYER_ASSIGNMENT (  '', '', ( #914 ) ) ;
#4522 = CARTESIAN_POINT ( 'NONE',  ( 8.370005009003978813, 7.147500832047211539, 32.36596039353565857 ) ) ;
#4523 = VECTOR ( 'NONE', #2789, 1000.000000000000000 ) ;
#4524 = AXIS2_PLACEMENT_3D ( 'NONE', #10, #4249, #1462 ) ;
#4525 = CARTESIAN_POINT ( 'NONE',  ( 6.586250505521797471, -10.16000000000000014, 2.540000505521796015 ) ) ;
#4526 = EDGE_LOOP ( 'NONE', ( #3576, #1693, #3856, #581 ) ) ;
#4527 = VERTEX_POINT ( 'NONE', #3964 ) ;
#4528 = AXIS2_PLACEMENT_3D ( 'NONE', #941, #2360, #3806 ) ;
#4529 = DIRECTION ( 'NONE',  ( -0.000000000000000000, -0.000000000000000000, -1.000000000000000000 ) ) ;
#4530 = VERTEX_POINT ( 'NONE', #412 ) ;
#4531 = FACE_OUTER_BOUND ( 'NONE', #334, .T. ) ;
#4532 = B_SPLINE_CURVE_WITH_KNOTS ( 'NONE', 3,
 ( #2890, #1095, #2466, #2445, #3542, #1073, #3630, #4315, #316, #3230, #3187, #3281, #1848, #4338, #1124, #4623, #3909, #686 ),
 .UNSPECIFIED., .F., .F.,
 ( 4, 2, 2, 2, 2, 2, 2, 2, 4 ),
 ( 0.005610428130223219997, 0.006311357680970762496, 0.007012287231718304994, 0.007713216782465847493, 0.008414146333213389992, 0.009115075883960932490, 0.009816005434708474989, 0.01051693498545601749, 0.01121786453620356172 ),
 .UNSPECIFIED. ) ;
#4533 = CARTESIAN_POINT ( 'NONE',  ( -14.03259314636827781, -2.691943933906732589, 34.72792442121545520 ) ) ;
#4534 = CARTESIAN_POINT ( 'NONE',  ( 13.83333314027809990, -3.573749167952787520, 32.12875308005140340 ) ) ;
#4535 = DIRECTION ( 'NONE',  ( 1.000000000000000000, 0.000000000000000000, 0.000000000000000000 ) ) ;
#4536 = CARTESIAN_POINT ( 'NONE',  ( -14.28749499099602183, -0.4675531348298848089, 28.79221039353566880 ) ) ;
#4537 = CARTESIAN_POINT ( 'NONE',  ( -8.369992765438045268, -6.393402013451325416, 31.86762445358908735 ) ) ;
#4538 = ORIENTED_EDGE ( 'NONE', *, *, #3593, .T. ) ;
#4539 = DIRECTION ( 'NONE',  ( -1.000000000000000000, -0.000000000000000000, -0.000000000000000000 ) ) ;
#4540 = AXIS2_PLACEMENT_3D ( 'NONE', #2162, #3601, #4331 ) ;
#4541 = CARTESIAN_POINT ( 'NONE',  ( -12.58715052442827442, 6.760359879724757270, 34.69836126359586359 ) ) ;
#4542 = ADVANCED_FACE ( 'NONE', ( #368, #737 ), #3216, .F. ) ;
#4543 = VERTEX_POINT ( 'NONE', #782 ) ;
#4544 = CARTESIAN_POINT ( 'NONE',  ( 14.17129034133389887, -1.872963726008691987, 38.78036386370911259 ) ) ;
#4545 = CARTESIAN_POINT ( 'NONE',  ( 7.234561953626996335E-06, 0.004097986548672528061, -10.04237554641092345 ) ) ;
#4546 = ADVANCED_FACE ( 'NONE', ( #4370 ), #2921, .T. ) ;
#4547 = ORIENTED_EDGE ( 'NONE', *, *, #3253, .T. ) ;
#4548 = ORIENTED_EDGE ( 'NONE', *, *, #3112, .F. ) ;
#4549 = LINE ( 'NONE', #3087, #2057 ) ;
#4550 = EDGE_LOOP ( 'NONE', ( #3465, #772, #426, #454 ) ) ;
#4551 = DIRECTION ( 'NONE',  ( 1.000000000000000000, 0.000000000000000000, 0.000000000000000000 ) ) ;
#4552 =( GEOMETRIC_REPRESENTATION_CONTEXT ( 3 ) GLOBAL_UNCERTAINTY_ASSIGNED_CONTEXT ( ( #3773 ) ) GLOBAL_UNIT_ASSIGNED_CONTEXT ( ( #3497, #956, #1024 ) ) REPRESENTATION_CONTEXT ( 'NONE', 'WORKASPACE' ) );
#4553 = DIRECTION ( 'NONE',  ( 1.000000000000000000, 0.000000000000000000, 0.000000000000000000 ) ) ;
#4554 = CARTESIAN_POINT ( 'NONE',  ( 7.620005009003977037, 12.08587093932537826, 39.51346039353565232 ) ) ;
#4555 = CARTESIAN_POINT ( 'NONE',  ( 7.234561953626996335E-06, 0.004097986548672528061, -10.04237554641092345 ) ) ;
#4556 = SURFACE_STYLE_FILL_AREA ( #3891 ) ;
#4557 = AXIS2_PLACEMENT_3D ( 'NONE', #1788, #2476, #390 ) ;
#4558 = CARTESIAN_POINT ( 'NONE',  ( -17.48249276543803532, -7.143402013451323640, 31.86762445358908735 ) ) ;
#4559 = PRODUCT_DEFINITION_SHAPE ( 'NONE', 'NONE',  #3297 ) ;
#4560 = CARTESIAN_POINT ( 'NONE',  ( 8.370005009003978813, -7.897499167952785726, 17.65096039353565160 ) ) ;
#4561 = CARTESIAN_POINT ( 'NONE',  ( 10.16000050552179701, -13.73374999999999879, 10.16000050552179701 ) ) ;
#4562 = CARTESIAN_POINT ( 'NONE',  ( -3.749999999999999556, 3.750000000000000000, 146.2500000000000000 ) ) ;
#4563 =( REPRESENTATION_RELATIONSHIP ('NONE','NONE', #4401, #1005 ) REPRESENTATION_RELATIONSHIP_WITH_TRANSFORMATION ( #1943 )SHAPE_REPRESENTATION_RELATIONSHIP( ) );
#4564 = EDGE_LOOP ( 'NONE', ( #2016, #2389, #4336, #3359, #863 ) ) ;
#4565 = AXIS2_PLACEMENT_3D ( 'NONE', #1567, #1915, #4073 ) ;
#4566 = CARTESIAN_POINT ( 'NONE',  ( 13.66253305200464929, -4.180199888423482335, 37.66696981337765493 ) ) ;
#4567 = EDGE_CURVE ( 'NONE', #2227, #1498, #3657, .T. ) ;
#4568 = DIRECTION ( 'NONE',  ( 0.000000000000000000, -1.000000000000000000, 0.000000000000000000 ) ) ;
#4569 = ORIENTED_EDGE ( 'NONE', *, *, #2269, .T. ) ;
#4570 = ORIENTED_EDGE ( 'NONE', *, *, #159, .T. ) ;
#4571 = TOROIDAL_SURFACE ( 'NONE', #967, 1.500000000000000000, 0.7500000000000000000 ) ;
#4572 = SURFACE_STYLE_USAGE ( .BOTH. , #4214 ) ;
#4573 = EDGE_CURVE ( 'NONE', #919, #2304, #2146, .T. ) ;
#4574 = ADVANCED_FACE ( 'NONE', ( #3990 ), #1158, .T. ) ;
#4575 = VERTEX_POINT ( 'NONE', #61 ) ;
#4576 = DIRECTION ( 'NONE',  ( 0.000000000000000000, 0.000000000000000000, 1.000000000000000000 ) ) ;
#4577 = LINE ( 'NONE', #4172, #3143 ) ;
#4578 = EDGE_CURVE ( 'NONE', #2506, #230, #1437, .T. ) ;
#4579 = CARTESIAN_POINT ( 'NONE',  ( -13.11702475164146264, -5.665798330090755286, 36.72925822850184829 ) ) ;
#4580 = CARTESIAN_POINT ( 'NONE',  ( 13.93190557999908918, -3.198157107824978418, 38.77513429737269490 ) ) ;
#4581 = DIRECTION ( 'NONE',  ( 1.000000000000000000, 0.000000000000000000, 0.000000000000000000 ) ) ;
#4582 = EDGE_CURVE ( 'NONE', #2359, #3460, #2222, .T. ) ;
#4583 = VECTOR ( 'NONE', #4427, 1000.000000000000000 ) ;
#4584 = DIRECTION ( 'NONE',  ( -1.000000000000000000, 8.673617379884035472E-17, 0.000000000000000000 ) ) ;
#4585 = LINE ( 'NONE', #298, #3433 ) ;
#4586 = CARTESIAN_POINT ( 'NONE',  ( 8.066546224052645542, -13.73374999999999524, 12.25345478699094670 ) ) ;
#4587 = LINE ( 'NONE', #545, #753 ) ;
#4588 = VECTOR ( 'NONE', #965, 1000.000000000000000 ) ;
#4589 = ORIENTED_EDGE ( 'NONE', *, *, #159, .F. ) ;
#4590 = CARTESIAN_POINT ( 'NONE',  ( -13.83927490936194360, 3.550949608386229528, 32.83276965945781711 ) ) ;
#4591 = TOROIDAL_SURFACE ( 'NONE', #2553, 6.397499999999999964, 0.7500000000000000000 ) ;
#4592 = CARTESIAN_POINT ( 'NONE',  ( 8.370005009003978813, 8.320472119090310841E-07, 32.36596039353565857 ) ) ;
#4593 = VERTEX_POINT ( 'NONE', #2833 ) ;
#4594 = ORIENTED_EDGE ( 'NONE', *, *, #183, .F. ) ;
#4595 = AXIS2_PLACEMENT_3D ( 'NONE', #2040, #2333, #4551 ) ;
#4596 = FILL_AREA_STYLE ('',( #3473 ) ) ;
#4597 = CARTESIAN_POINT ( 'NONE',  ( 2.540000505521796015, -2.539999999999999591, 3.040000505521795571 ) ) ;
#4598 = PRODUCT ( 'Part 134_Varsay\X2\0131\X0\lan', 'Part 134_Varsay\X2\0131\X0\lan', '', ( #758 ) ) ;
#4599 = ORIENTED_EDGE ( 'NONE', *, *, #1799, .F. ) ;
#4600 = DIRECTION ( 'NONE',  ( 1.076498916035107621E-16, -1.000000000000000000, 0.000000000000000000 ) ) ;
#4601 = ORIENTED_EDGE ( 'NONE', *, *, #2409, .F. ) ;
#4602 = CARTESIAN_POINT ( 'NONE',  ( -8.369994990996019624, 8.320472137110901854E-07, 32.36596039353565857 ) ) ;
#4603 = EDGE_CURVE ( 'NONE', #2813, #1351, #1023, .T. ) ;
#4604 = CARTESIAN_POINT ( 'NONE',  ( -11.96599325036756589, 7.811730032674823576, 17.15262445358908039 ) ) ;
#4605 = DIRECTION ( 'NONE',  ( 0.000000000000000000, 0.000000000000000000, 1.000000000000000000 ) ) ;
#4606 = DIRECTION ( 'NONE',  ( -0.000000000000000000, -1.000000000000000000, -0.000000000000000000 ) ) ;
#4607 = LINE ( 'NONE', #4558, #1377 ) ;
#4608 = EDGE_CURVE ( 'NONE', #4593, #2966, #2007, .T. ) ;
#4609 = CARTESIAN_POINT ( 'NONE',  ( 14.28750500900398102, -0.2356504121955460829, 35.93971039353566965 ) ) ;
#4610 = DIRECTION ( 'NONE',  ( -0.000000000000000000, -0.000000000000000000, -1.000000000000000000 ) ) ;
#4611 = DIRECTION ( 'NONE',  ( 0.000000000000000000, 0.000000000000000000, 1.000000000000000000 ) ) ;
#4612 = LINE ( 'NONE', #3552, #4523 ) ;
#4613 = ORIENTED_EDGE ( 'NONE', *, *, #4429, .F. ) ;
#4614 = CARTESIAN_POINT ( 'NONE',  ( 13.93190780555705999, -3.194059953323518108, 38.27679835742612369 ) ) ;
#4615 = CIRCLE ( 'NONE', #2949, 14.28750000000000142 ) ;
#4616 = CARTESIAN_POINT ( 'NONE',  ( -3.573742765438046476, 0.004097986548672528061, 17.16762445358907385 ) ) ;
#4617 = ORIENTED_EDGE ( 'NONE', *, *, #4603, .F. ) ;
#4618 = EDGE_LOOP ( 'NONE', ( #875, #2863, #3276, #2537 ) ) ;
#4619 = EDGE_CURVE ( 'NONE', #2728, #3496, #1107, .T. ) ;
#4620 = VERTEX_POINT ( 'NONE', #714 ) ;
#4621 = CARTESIAN_POINT ( 'NONE',  ( 3.749999999999999556, -3.750000000000000888, 18.74999999999999645 ) ) ;
#4622 = ORIENTED_EDGE ( 'NONE', *, *, #2701, .F. ) ;
#4623 = CARTESIAN_POINT ( 'NONE',  ( -14.28158774459093117, 0.4750311026362873390, 28.31727528644927006 ) ) ;
#4624 = DIRECTION ( 'NONE',  ( -2.428612866367729613E-17, 1.000000000000000000, -1.249000902703301108E-16 ) ) ;
#4625 = CARTESIAN_POINT ( 'NONE',  ( -12.76961707278682923, -6.411760650040047693, 35.55869424641612397 ) ) ;
#4626 = ADVANCED_FACE ( 'NONE', ( #3236 ), #12, .F. ) ;
#4627 = CARTESIAN_POINT ( 'NONE',  ( -7.619994990996021400, -6.397499167952784838, 18.40096039353565160 ) ) ;
#4628 = DIRECTION ( 'NONE',  ( 0.000000000000000000, 0.000000000000000000, 1.000000000000000000 ) ) ;
#4629 = ORIENTED_EDGE ( 'NONE', *, *, #600, .T. ) ;
#4630 = PLANE ( 'NONE',  #1307 ) ;
#4631 = DIRECTION ( 'NONE',  ( 0.000000000000000000, -1.000000000000000000, 0.000000000000000000 ) ) ;
#4632 = PLANE ( 'NONE',  #2320 ) ;
#4633 = AXIS2_PLACEMENT_3D ( 'NONE', #3826, #3895, #3145 ) ;
#4634 = DIRECTION ( 'NONE',  ( 1.000000000000000000, -1.076498916035107621E-16, 0.000000000000000000 ) ) ;
#4635 = EDGE_CURVE ( 'NONE', #2793, #2774, #1187, .T. ) ;
#4636 = VERTEX_POINT ( 'NONE', #2645 ) ;
#4637 = CARTESIAN_POINT ( 'NONE',  ( 13.83079258162059588, -3.601903900406878911, 38.05628366828691611 ) ) ;
#4638 = DIRECTION ( 'NONE',  ( -0.7071067811865449082, 8.659560562354902043E-17, 0.7071067811865501263 ) ) ;
#4639 = CIRCLE ( 'NONE', #1910, 4.762499999999999289 ) ;
#4640 = ADVANCED_FACE ( 'NONE', ( #1551 ), #1601, .F. ) ;
#4641 = EDGE_LOOP ( 'NONE', ( #241, #48, #1983 ) ) ;
#4642 = AXIS2_PLACEMENT_3D ( 'NONE', #175, #1620, #3037 ) ;
#4643 = ORIENTED_EDGE ( 'NONE', *, *, #177, .T. ) ;
#4644 = ADVANCED_FACE ( 'NONE', ( #2945 ), #3679, .T. ) ;
#4645 =( NAMED_UNIT ( * ) PLANE_ANGLE_UNIT ( ) SI_UNIT ( $, .RADIAN. ) );
#4646 = VECTOR ( 'NONE', #3686, 1000.000000000000000 ) ;
#4647 = EDGE_LOOP ( 'NONE', ( #96, #1119 ) ) ;
#4648 = CARTESIAN_POINT ( 'NONE',  ( 3.040000505521796015, -3.039999999999999591, 17.28000050552179445 ) ) ;
#4649 = VERTEX_POINT ( 'NONE', #4393 ) ;
#4650 = NEXT_ASSEMBLY_USAGE_OCCURRENCE ( 'NAUO1', ' ', ' ', #1350, #500, $ ) ;
#4651 = NEXT_ASSEMBLY_USAGE_OCCURRENCE ( 'NAUO2', ' ', ' ', #1350, #3694, $ ) ;
#4652 = NEXT_ASSEMBLY_USAGE_OCCURRENCE ( 'NAUO3', ' ', ' ', #1350, #1640, $ ) ;
#4653 = NEXT_ASSEMBLY_USAGE_OCCURRENCE ( 'NAUO4', ' ', ' ', #1350, #3981, $ ) ;
#4654 = NEXT_ASSEMBLY_USAGE_OCCURRENCE ( 'NAUO5', ' ', ' ', #1350, #3297, $ ) ;
#4655 = NEXT_ASSEMBLY_USAGE_OCCURRENCE ( 'NAUO6', ' ', ' ', #1350, #3297, $ ) ;
#4656 = NEXT_ASSEMBLY_USAGE_OCCURRENCE ( 'NAUO7', ' ', ' ', #1350, #14, $ ) ;
#4657 = NEXT_ASSEMBLY_USAGE_OCCURRENCE ( 'NAUO8', ' ', ' ', #1350, #3694, $ ) ;
#4658 = NEXT_ASSEMBLY_USAGE_OCCURRENCE ( 'NAUO9', ' ', ' ', #1350, #1640, $ ) ;
#4659 = NEXT_ASSEMBLY_USAGE_OCCURRENCE ( 'NAUO10', ' ', ' ', #1350, #3297, $ ) ;
#4660 = NEXT_ASSEMBLY_USAGE_OCCURRENCE ( 'NAUO11', ' ', ' ', #1350, #3981, $ ) ;
#4661 = NEXT_ASSEMBLY_USAGE_OCCURRENCE ( 'NAUO12', ' ', ' ', #1350, #500, $ ) ;
#4662 = NEXT_ASSEMBLY_USAGE_OCCURRENCE ( 'NAUO13', ' ', ' ', #1350, #3297, $ ) ;
ENDSEC;
END-ISO-10303-21;
